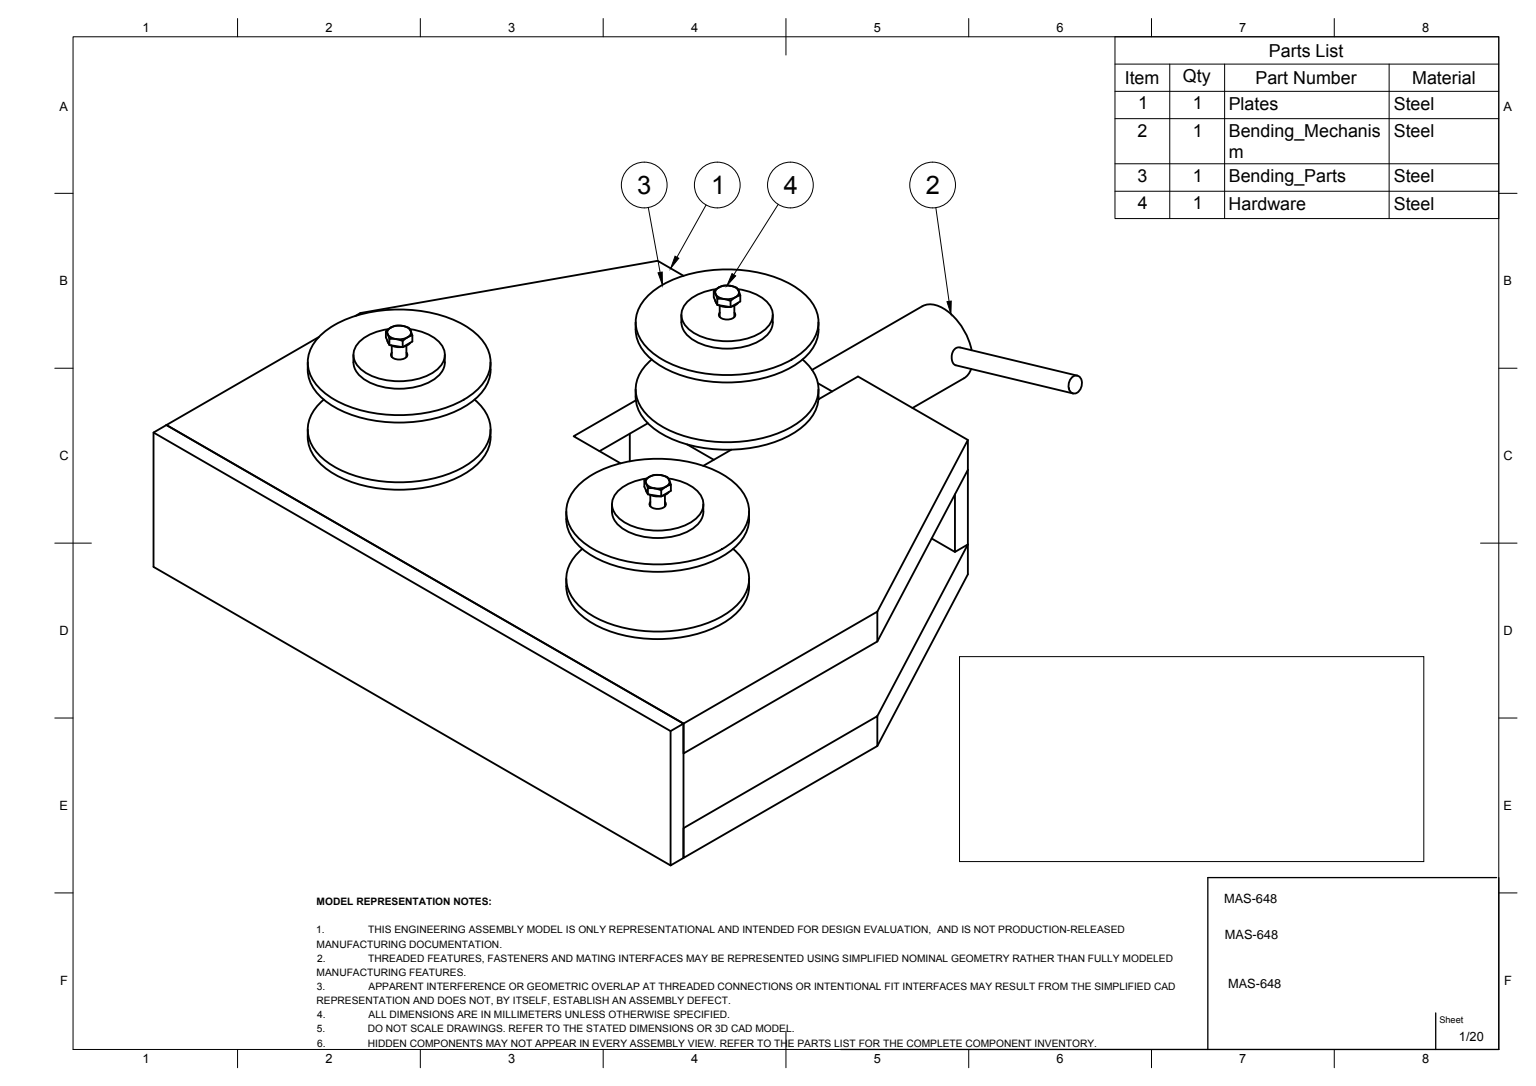
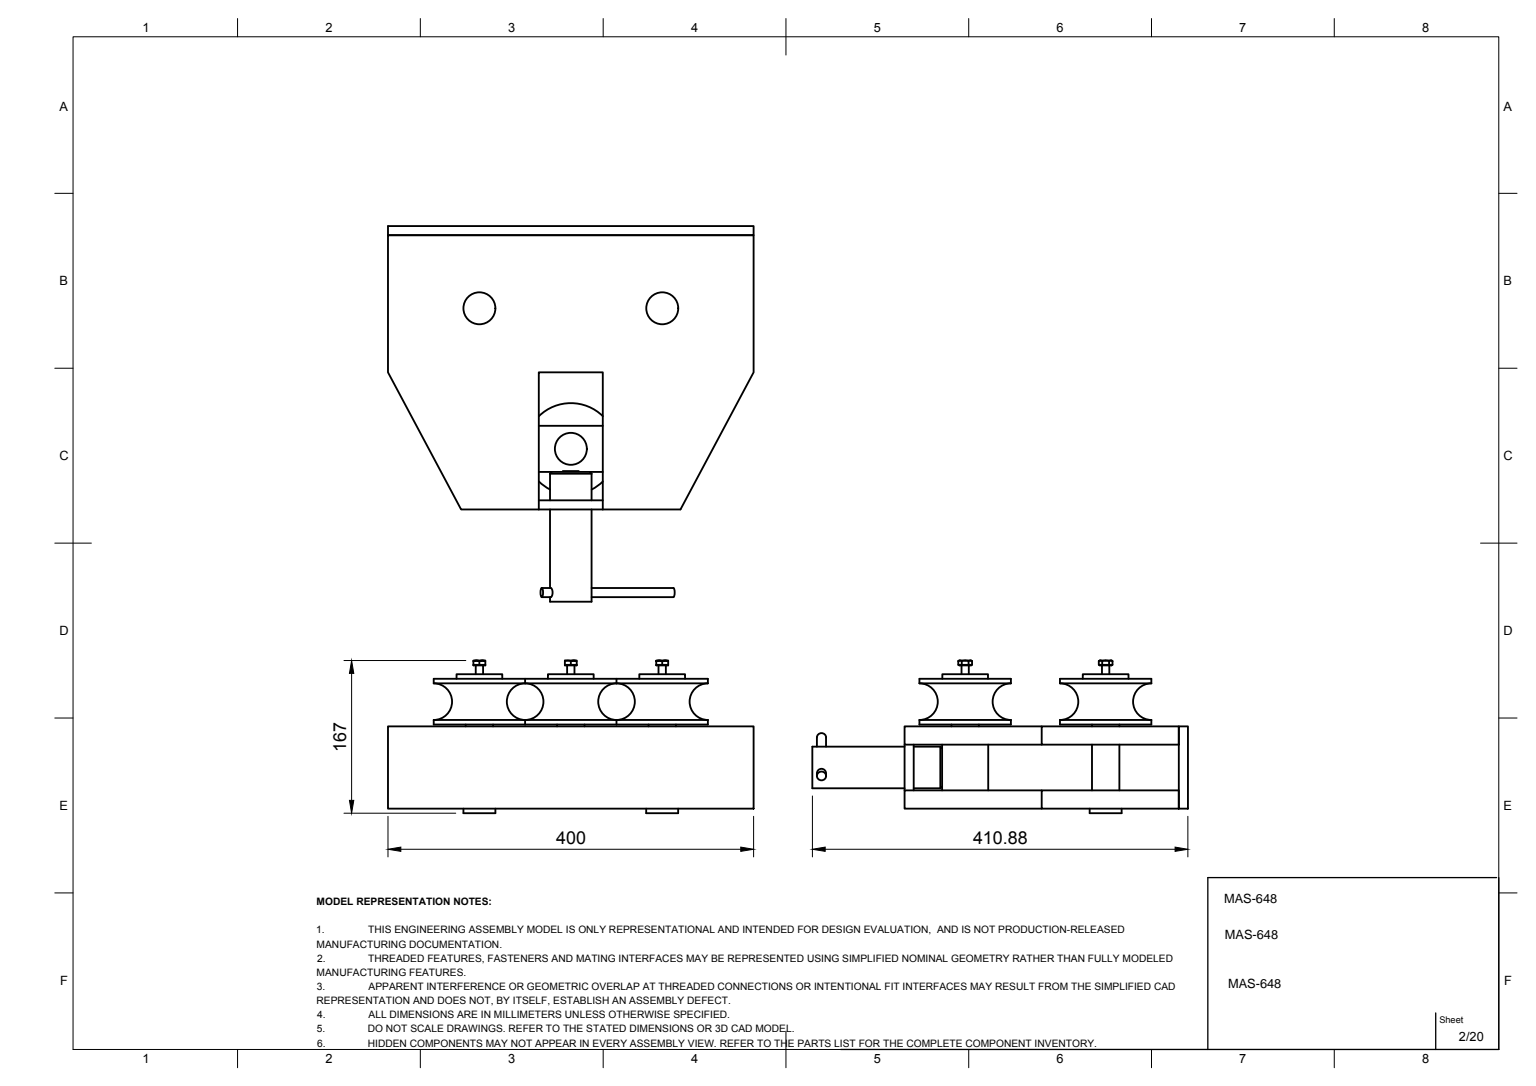
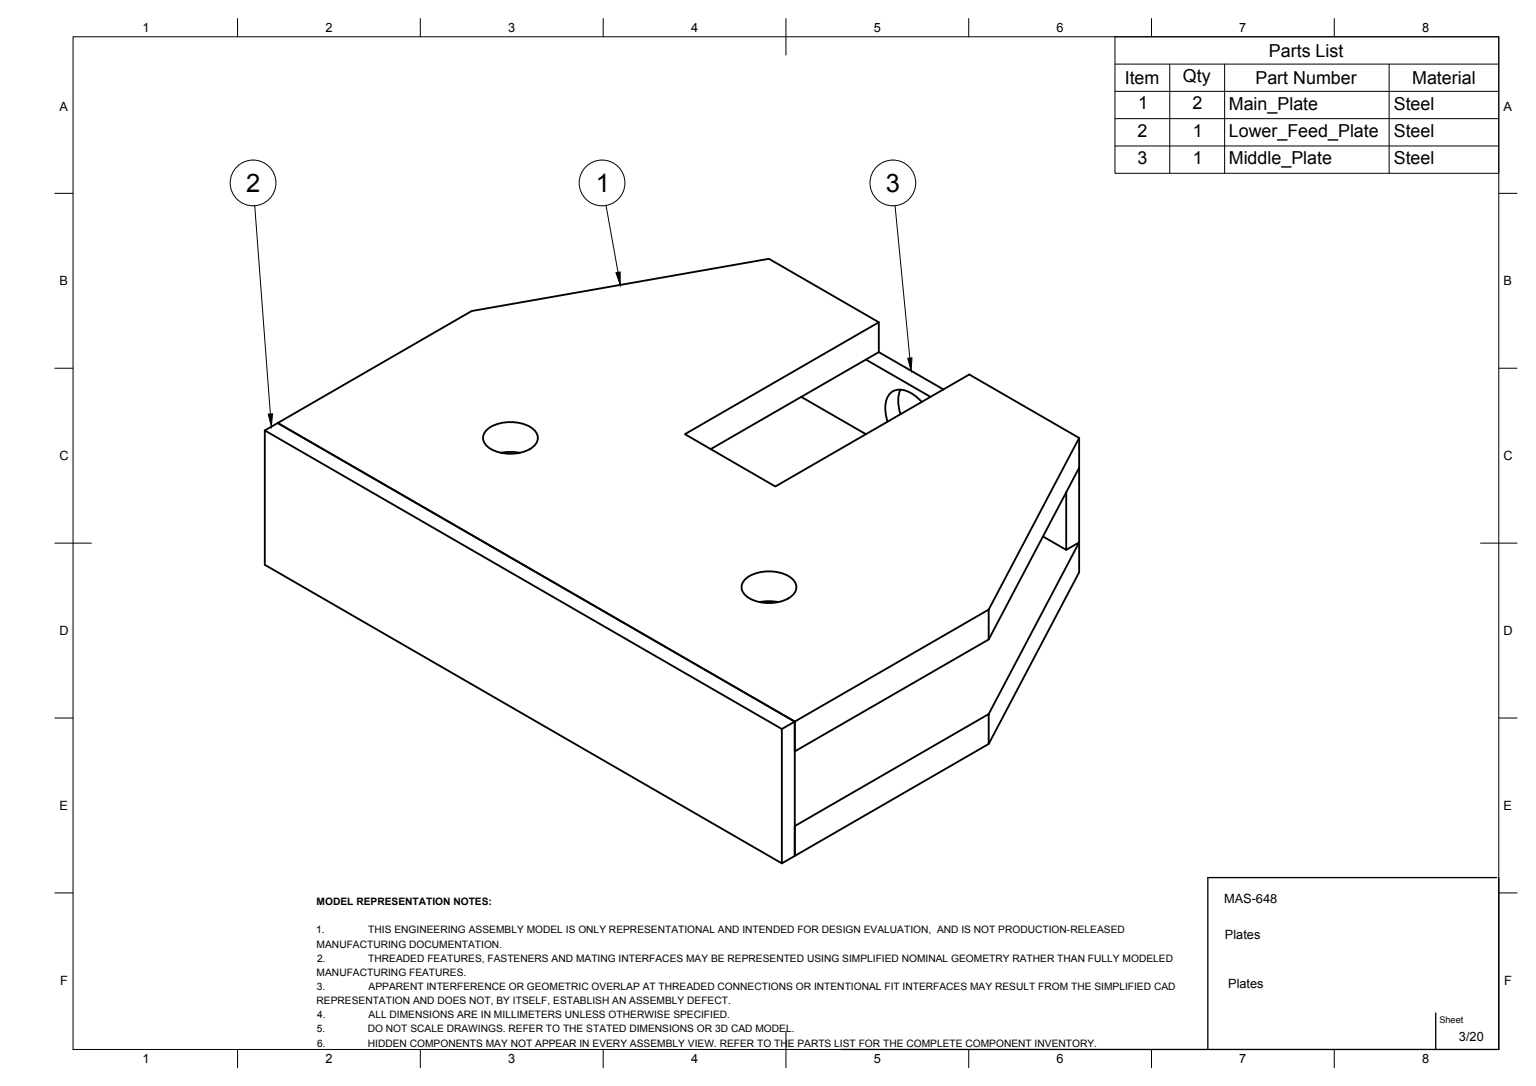
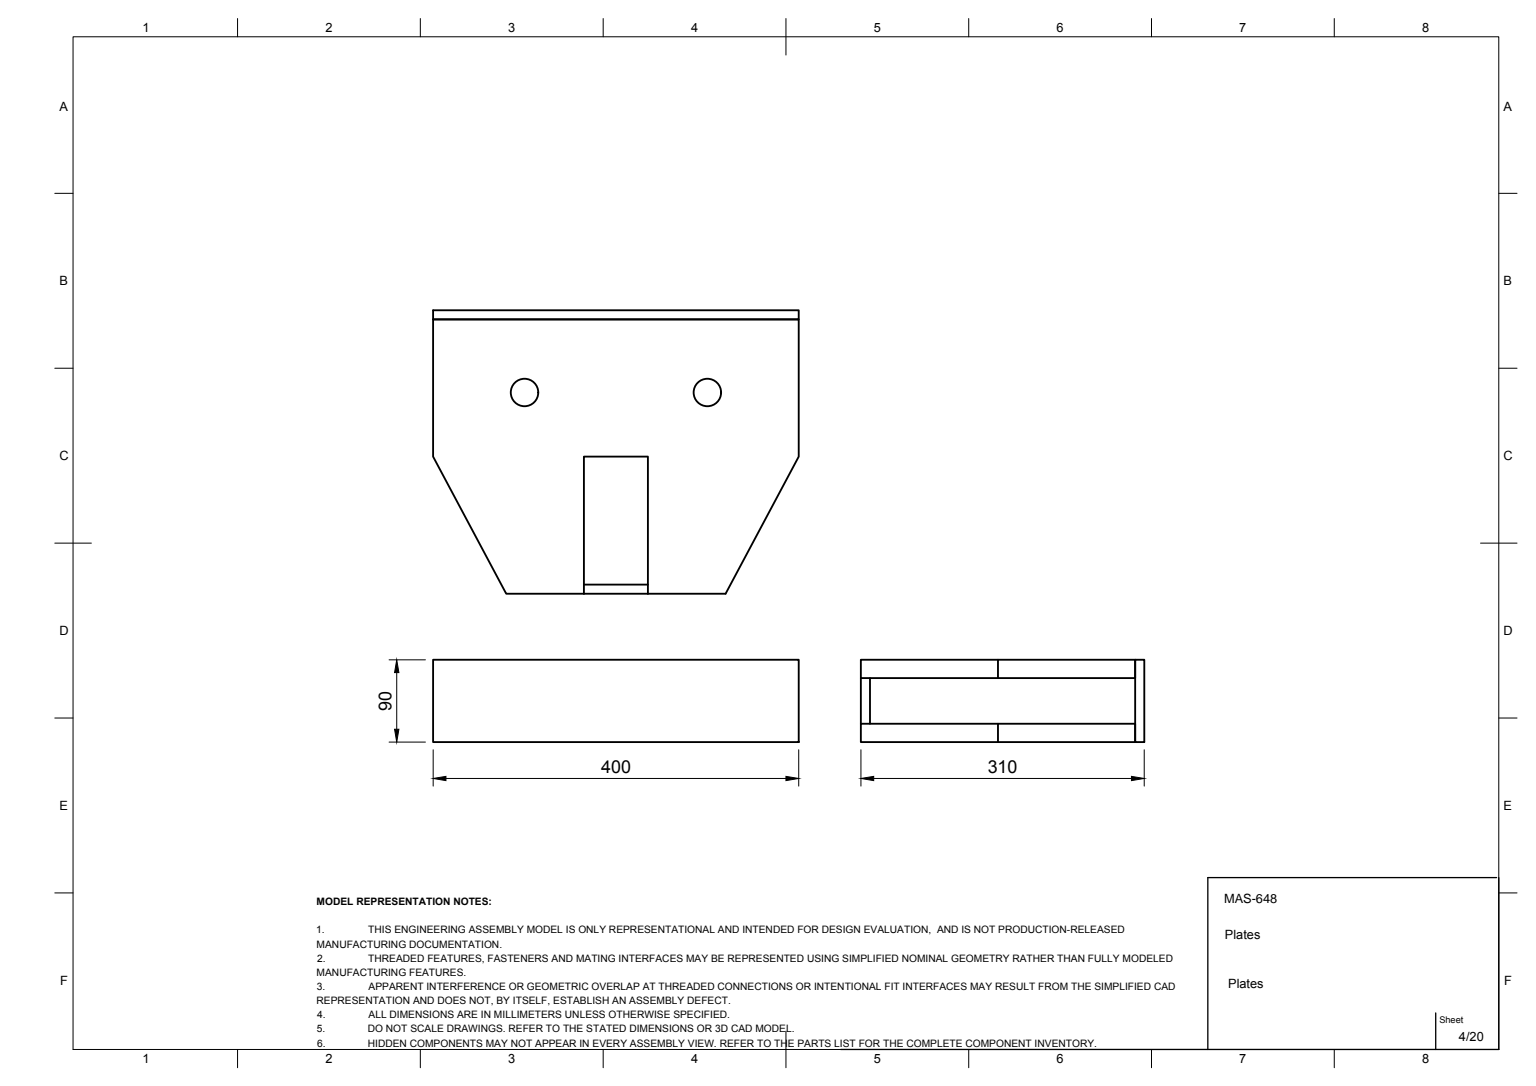
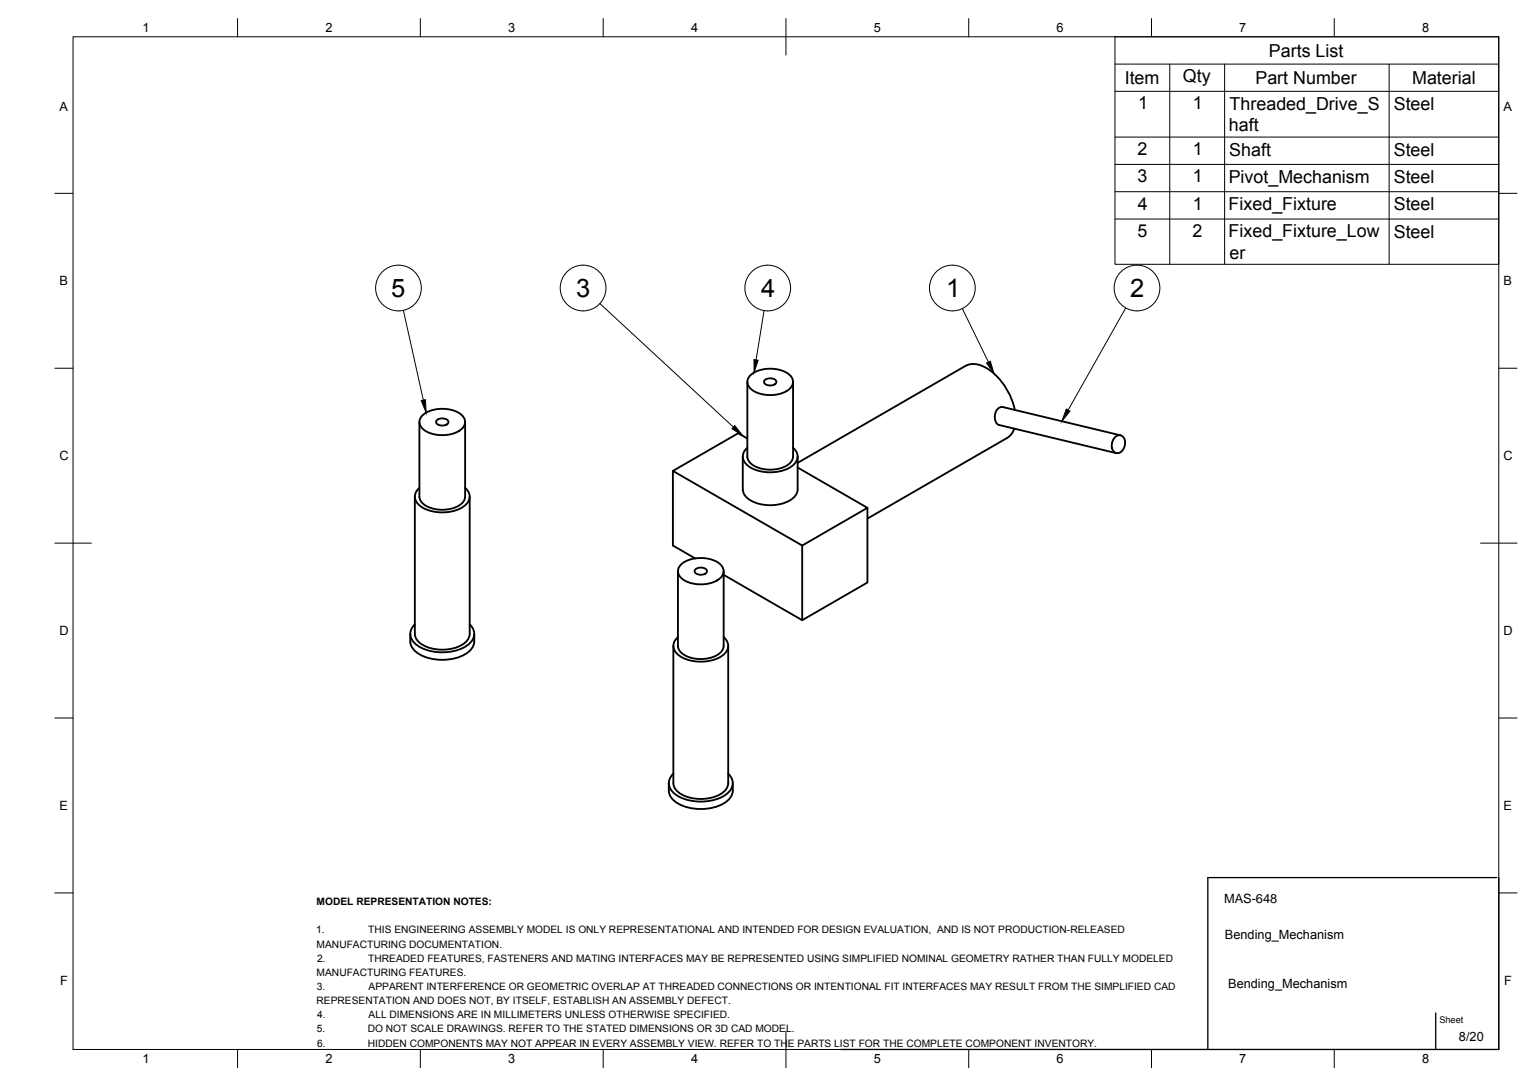
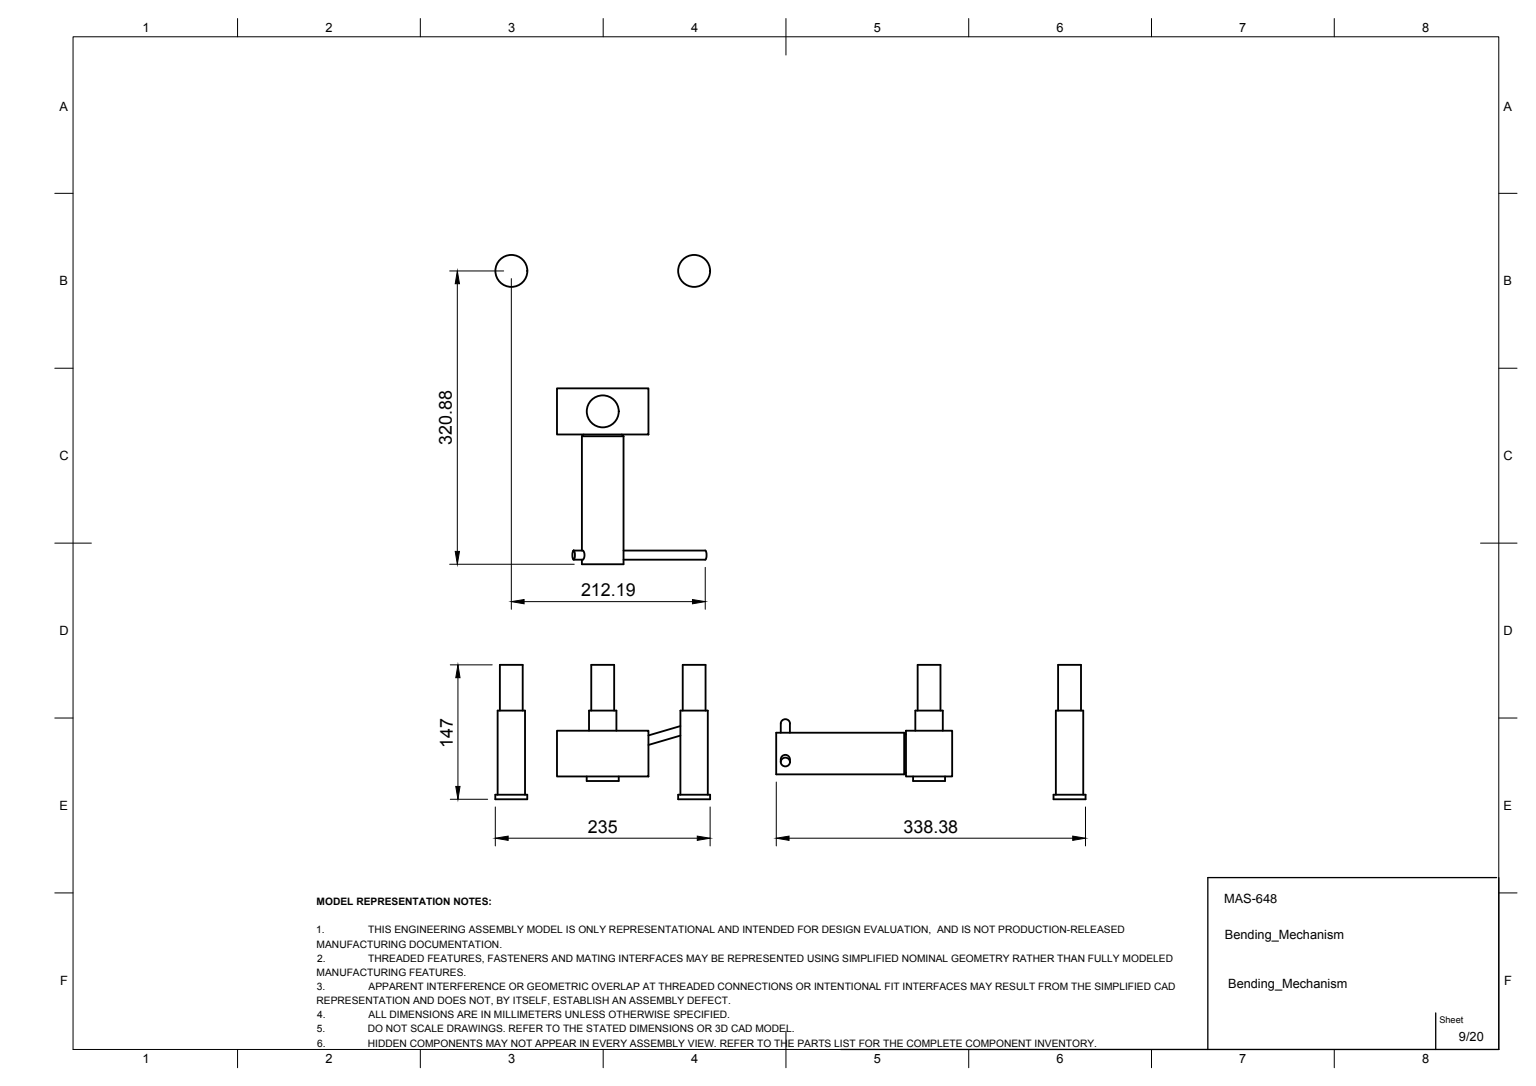
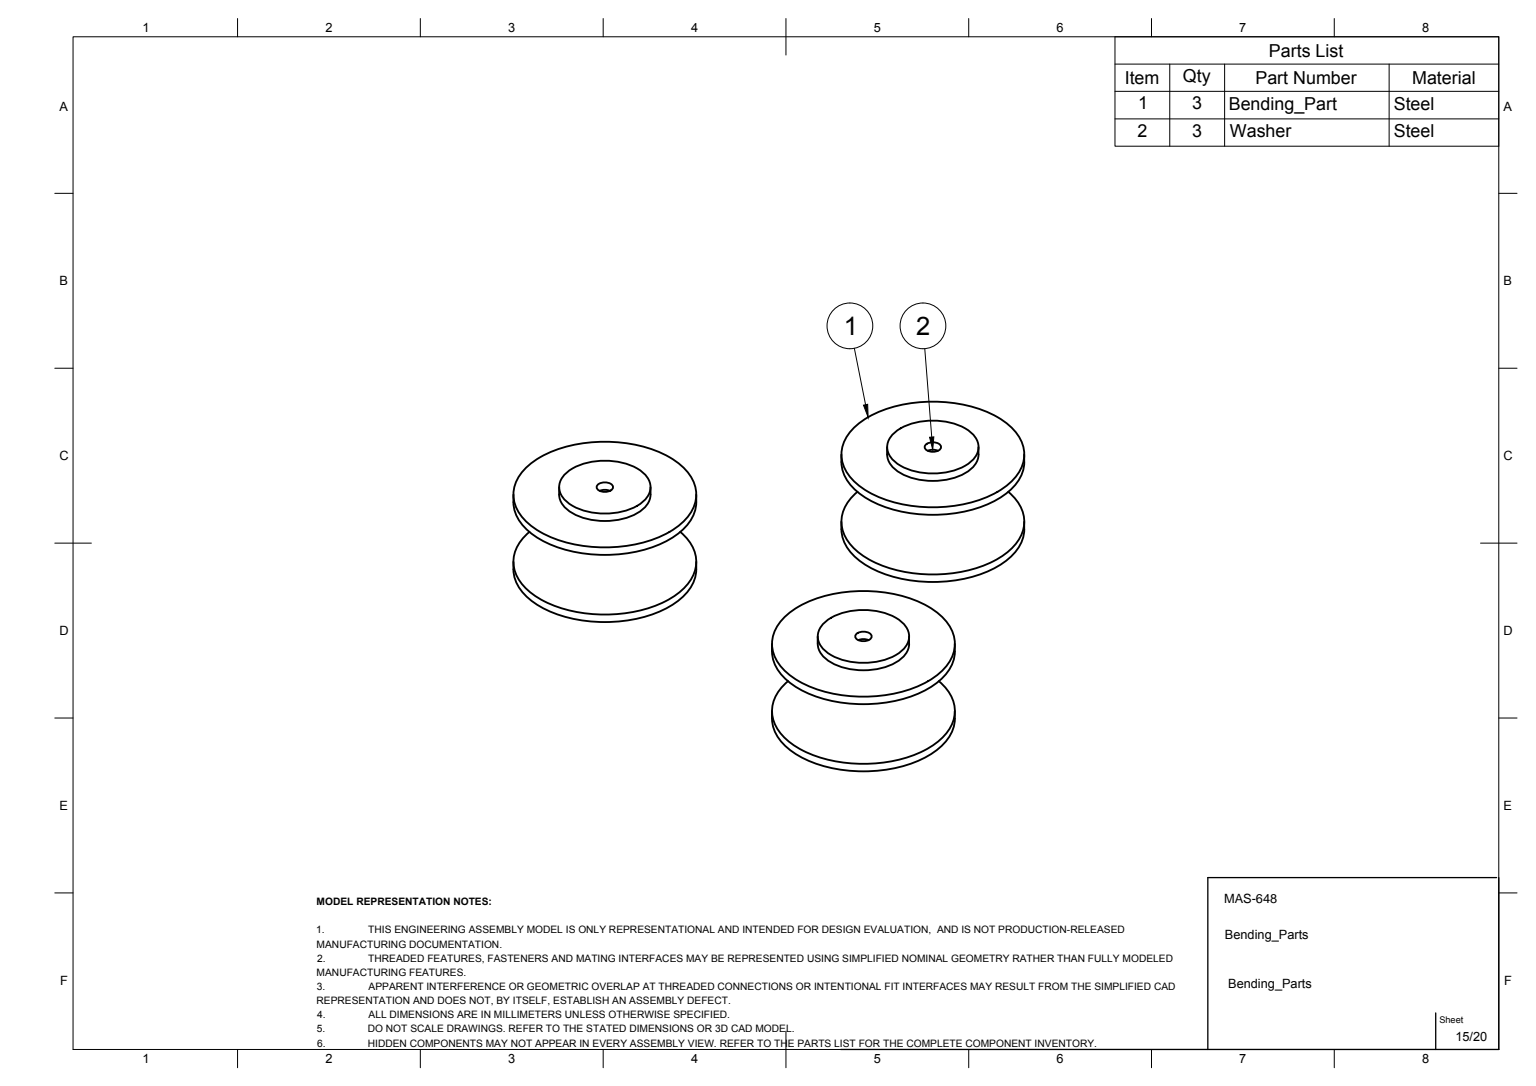
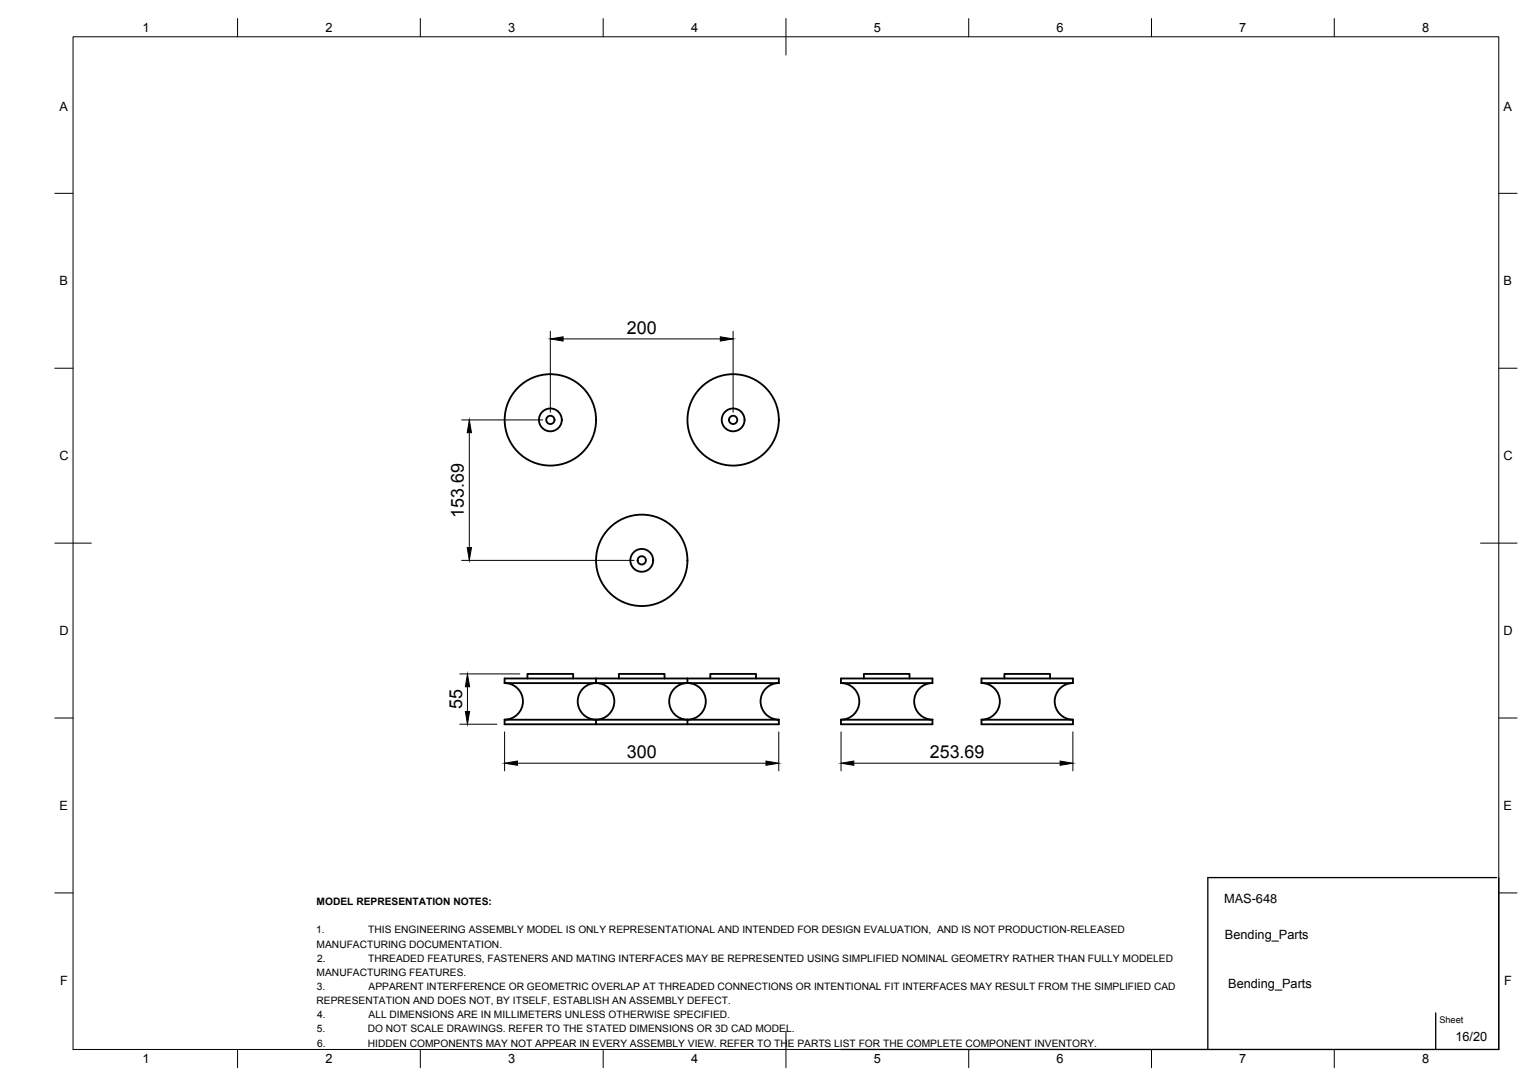
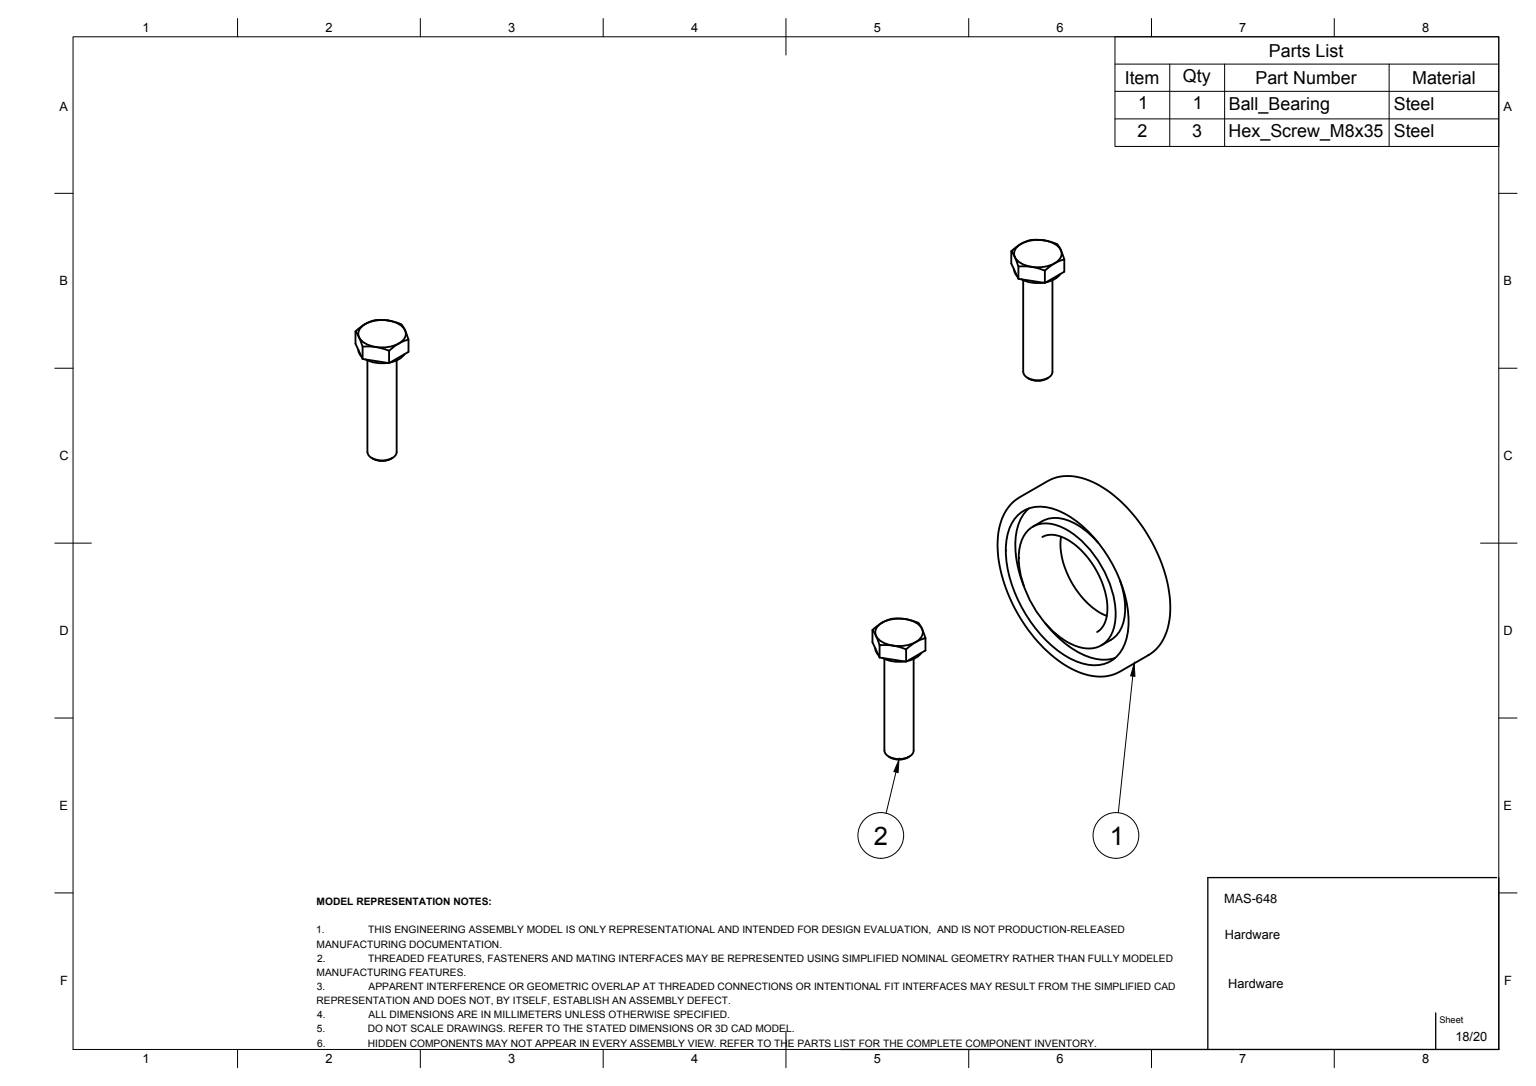
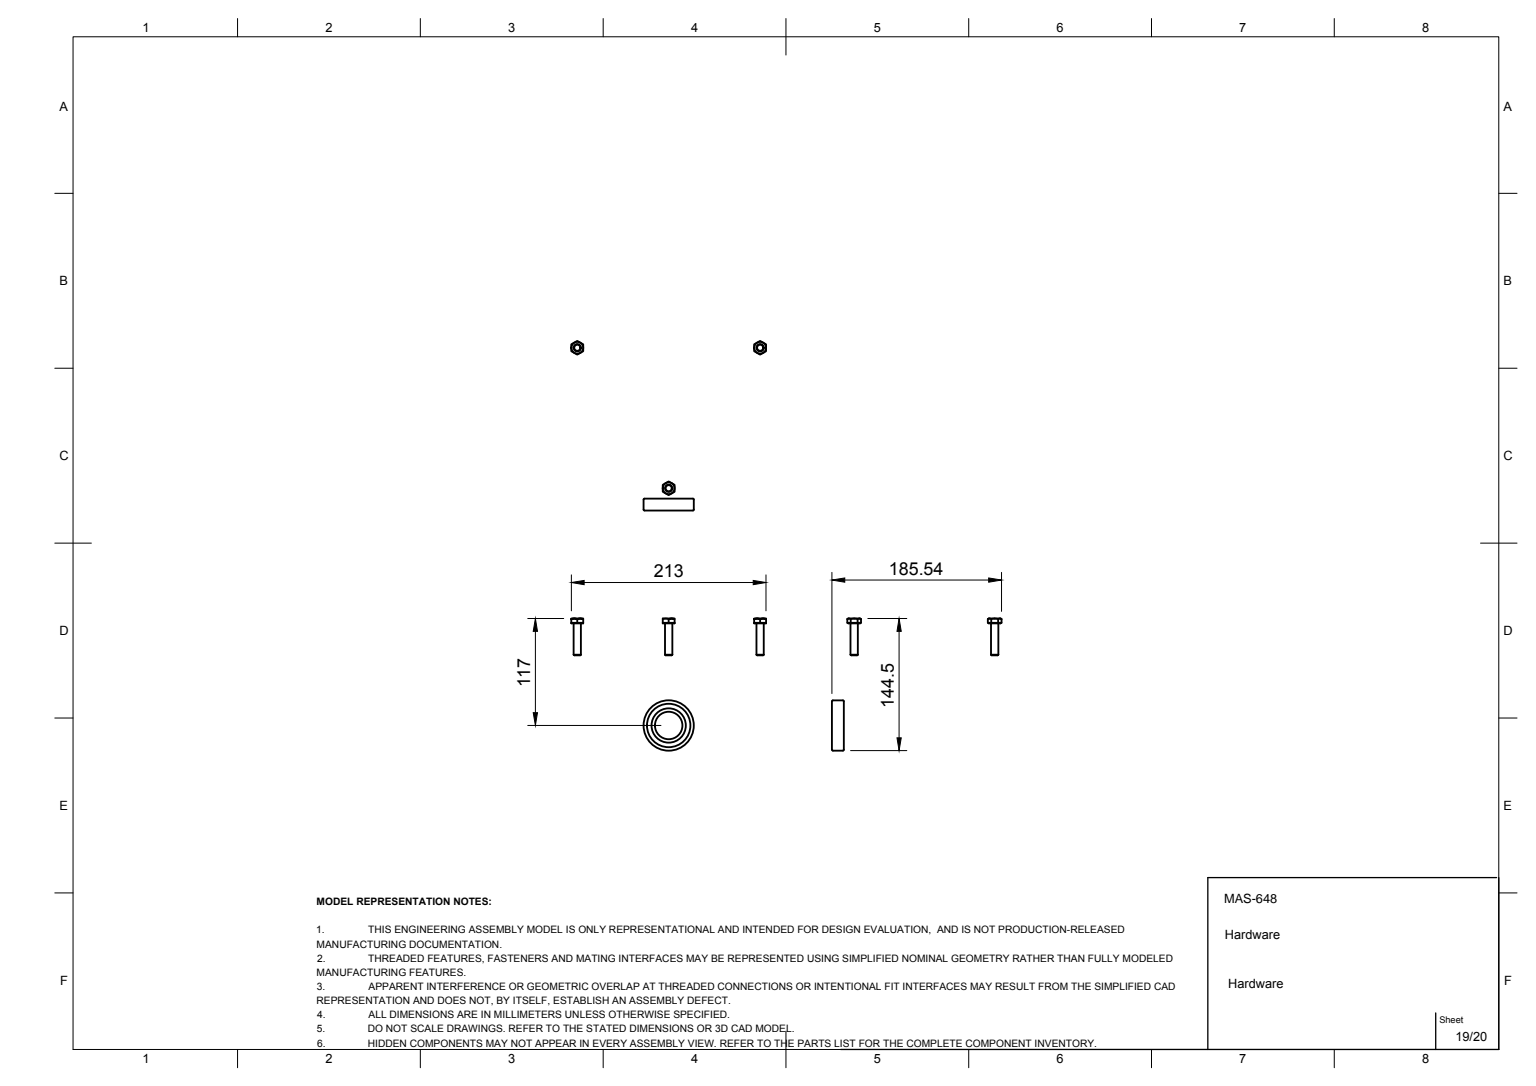
ISO-10303-21;
HEADER;
FILE_DESCRIPTION((''),'2;1');
FILE_NAME('MAS-648','2026-10-09T12:47:58-07:00',(''),(''),'','','');
FILE_SCHEMA (('AUTOMOTIVE_DESIGN { 1 0 10303 214 3 1 1 }'));
ENDSEC;
DATA;
#10 = MECHANICAL_DESIGN_GEOMETRIC_PRESENTATION_REPRESENTATION('',(#310,#311,
#312,#313,#314,#315,#316,#317,#318,#319,#320,#321),#3475) ;
#11 = (
BOUNDED_CURVE()
B_SPLINE_CURVE(2,(#3374,#3375,#3376),.UNSPECIFIED.,.F.,.F.)
B_SPLINE_CURVE_WITH_KNOTS((3,3),(-1.6071868741402,-0.951706480249473),
 .UNSPECIFIED.)
CURVE()
GEOMETRIC_REPRESENTATION_ITEM()
RATIONAL_B_SPLINE_CURVE((1.7594376617802,1.7594376617802,1.63311572113257))
REPRESENTATION_ITEM('')
) ;
#12 = (
BOUNDED_CURVE()
B_SPLINE_CURVE(2,(#3377,#3378,#3379),.UNSPECIFIED.,.F.,.F.)
B_SPLINE_CURVE_WITH_KNOTS((3,3),(-2.26266726803093,-1.6071868741402),
 .UNSPECIFIED.)
CURVE()
GEOMETRIC_REPRESENTATION_ITEM()
RATIONAL_B_SPLINE_CURVE((1.63311572113257,1.7594376617802,1.7594376617802))
REPRESENTATION_ITEM('')
) ;
#13 = (
BOUNDED_CURVE()
B_SPLINE_CURVE(2,(#3382,#3383,#3384),.UNSPECIFIED.,.F.,.F.)
B_SPLINE_CURVE_WITH_KNOTS((3,3),(-1.6071868741402,-0.951706480249475),
 .UNSPECIFIED.)
CURVE()
GEOMETRIC_REPRESENTATION_ITEM()
RATIONAL_B_SPLINE_CURVE((1.7594376617802,1.7594376617802,1.63311572113257))
REPRESENTATION_ITEM('')
) ;
#14 = (
BOUNDED_CURVE()
B_SPLINE_CURVE(2,(#3385,#3386,#3387),.UNSPECIFIED.,.F.,.F.)
B_SPLINE_CURVE_WITH_KNOTS((3,3),(-2.26266726803093,-1.6071868741402),
 .UNSPECIFIED.)
CURVE()
GEOMETRIC_REPRESENTATION_ITEM()
RATIONAL_B_SPLINE_CURVE((1.63311572113257,1.7594376617802,1.7594376617802))
REPRESENTATION_ITEM('')
) ;
#15 = (
BOUNDED_CURVE()
B_SPLINE_CURVE(2,(#3390,#3391,#3392),.UNSPECIFIED.,.F.,.F.)
B_SPLINE_CURVE_WITH_KNOTS((3,3),(-2.26266726803093,-1.6071868741402),
 .UNSPECIFIED.)
CURVE()
GEOMETRIC_REPRESENTATION_ITEM()
RATIONAL_B_SPLINE_CURVE((1.63311572113257,1.7594376617802,1.7594376617802))
REPRESENTATION_ITEM('')
) ;
#16 = (
BOUNDED_CURVE()
B_SPLINE_CURVE(2,(#3393,#3394,#3395),.UNSPECIFIED.,.F.,.F.)
B_SPLINE_CURVE_WITH_KNOTS((3,3),(-1.6071868741402,-0.951706480249475),
 .UNSPECIFIED.)
CURVE()
GEOMETRIC_REPRESENTATION_ITEM()
RATIONAL_B_SPLINE_CURVE((1.7594376617802,1.7594376617802,1.63311572113257))
REPRESENTATION_ITEM('')
) ;
#17 = (
BOUNDED_CURVE()
B_SPLINE_CURVE(2,(#3398,#3399,#3400),.UNSPECIFIED.,.F.,.F.)
B_SPLINE_CURVE_WITH_KNOTS((3,3),(-2.26266726803093,-1.6071868741402),
 .UNSPECIFIED.)
CURVE()
GEOMETRIC_REPRESENTATION_ITEM()
RATIONAL_B_SPLINE_CURVE((1.63311572113257,1.7594376617802,1.7594376617802))
REPRESENTATION_ITEM('')
) ;
#18 = (
BOUNDED_CURVE()
B_SPLINE_CURVE(2,(#3401,#3402,#3403),.UNSPECIFIED.,.F.,.F.)
B_SPLINE_CURVE_WITH_KNOTS((3,3),(-1.6071868741402,-0.951706480249475),
 .UNSPECIFIED.)
CURVE()
GEOMETRIC_REPRESENTATION_ITEM()
RATIONAL_B_SPLINE_CURVE((1.7594376617802,1.7594376617802,1.63311572113257))
REPRESENTATION_ITEM('')
) ;
#19 = (
BOUNDED_CURVE()
B_SPLINE_CURVE(2,(#3406,#3407,#3408),.UNSPECIFIED.,.F.,.F.)
B_SPLINE_CURVE_WITH_KNOTS((3,3),(-1.6071868741402,-0.951706480249475),
 .UNSPECIFIED.)
CURVE()
GEOMETRIC_REPRESENTATION_ITEM()
RATIONAL_B_SPLINE_CURVE((1.7594376617802,1.7594376617802,1.63311572113257))
REPRESENTATION_ITEM('')
) ;
#20 = (
BOUNDED_CURVE()
B_SPLINE_CURVE(2,(#3409,#3410,#3411),.UNSPECIFIED.,.F.,.F.)
B_SPLINE_CURVE_WITH_KNOTS((3,3),(-2.26266726803093,-1.6071868741402),
 .UNSPECIFIED.)
CURVE()
GEOMETRIC_REPRESENTATION_ITEM()
RATIONAL_B_SPLINE_CURVE((1.63311572113258,1.7594376617802,1.7594376617802))
REPRESENTATION_ITEM('')
) ;
#21 = (
BOUNDED_CURVE()
B_SPLINE_CURVE(2,(#3414,#3415,#3416),.UNSPECIFIED.,.F.,.F.)
B_SPLINE_CURVE_WITH_KNOTS((3,3),(-2.26266726803093,-1.6071868741402),
 .UNSPECIFIED.)
CURVE()
GEOMETRIC_REPRESENTATION_ITEM()
RATIONAL_B_SPLINE_CURVE((1.63311572113257,1.7594376617802,1.7594376617802))
REPRESENTATION_ITEM('')
) ;
#22 = (
BOUNDED_CURVE()
B_SPLINE_CURVE(2,(#3417,#3418,#3419),.UNSPECIFIED.,.F.,.F.)
B_SPLINE_CURVE_WITH_KNOTS((3,3),(-1.6071868741402,-0.951706480249472),
 .UNSPECIFIED.)
CURVE()
GEOMETRIC_REPRESENTATION_ITEM()
RATIONAL_B_SPLINE_CURVE((1.7594376617802,1.7594376617802,1.63311572113257))
REPRESENTATION_ITEM('')
) ;
#23 = TOROIDAL_SURFACE('',#2087,50.,20.) ;
#24 = TOROIDAL_SURFACE('',#2119,26.5,1.) ;
#25 = TOROIDAL_SURFACE('',#2125,26.5,1.) ;
#26 = TOROIDAL_SURFACE('',#2136,21.25,3.75) ;
#27 = TOROIDAL_SURFACE('',#2140,16.,1.) ;
#28 = TOROIDAL_SURFACE('',#2146,16.,1.) ;
#29 = TOROIDAL_SURFACE('',#2155,21.25,3.75) ;
#30 = TOROIDAL_SURFACE('',#2162,4.4,0.4) ;
#31 = CONICAL_SURFACE('',#2014,22.7551020408163,0.785398163397443) ;
#32 = CONICAL_SURFACE('',#2047,3.39999999999999,1.02974425867665) ;
#33 = CONICAL_SURFACE('',#2065,3.39999999999999,1.02974425867665) ;
#34 = CONICAL_SURFACE('',#2175,3.3095,0.785398163397441) ;
#35 = CONICAL_SURFACE('',#2194,6.5,1.0471975511966) ;
#36 = CONICAL_SURFACE('',#2195,6.5,1.0471975511966) ;
#37 = CONICAL_SURFACE('',#2196,6.5,1.0471975511966) ;
#38 = CONICAL_SURFACE('',#2197,6.5,1.0471975511966) ;
#39 = CONICAL_SURFACE('',#2198,6.5,1.0471975511966) ;
#40 = CONICAL_SURFACE('',#2199,6.5,1.0471975511966) ;
#41 = B_SPLINE_CURVE_WITH_KNOTS('',3,(#2969,#2970,#2971,#2972,#2973,#2974,
#2975,#2976,#2977,#2978,#2979,#2980,#2981,#2982,#2983,#2984,#2985,#2986,
#2987),.UNSPECIFIED.,.F.,.F.,(4,2,2,2,3,2,2,2,4),(-0.756034971359867,-0.567034005964369,
-0.378033040568871,-0.189016520284436,0.,0.189016520284436,0.378033040568871,
0.567034005964369,0.756034971359867),.UNSPECIFIED.) ;
#42 = B_SPLINE_CURVE_WITH_KNOTS('',3,(#2989,#2990,#2991,#2992,#2993,#2994,
#2995,#2996,#2997,#2998),.UNSPECIFIED.,.F.,.F.,(4,2,2,2,4),(0.756034971359867,
0.945035936755365,1.13403690215086,1.3230534224353,1.51206994271973),
 .UNSPECIFIED.) ;
#43 = B_SPLINE_CURVE_WITH_KNOTS('',3,(#3001,#3002,#3003,#3004,#3005,#3006,
#3007,#3008,#3009,#3010,#3011,#3012,#3013,#3014,#3015,#3016,#3017,#3018,
#3019,#3020,#3021,#3022,#3023,#3024,#3025,#3026,#3027,#3028,#3029,#3030,
#3031,#3032,#3033,#3034),.UNSPECIFIED.,.T.,.F.,(4,2,2,2,2,2,2,2,2,2,2,2,
2,2,2,2,4),(-3.02413988543947,-2.83512336515503,-2.6461068448706,-2.4571058794751,
-2.2681049140796,-2.0791039486841,-1.8901029832886,-1.70108646300417,-1.51206994271973,
-1.3230534224353,-1.13403690215086,-0.945035936755364,-0.756034971359867,
-0.567034005964369,-0.378033040568871,-0.189016520284436,0.),
 .UNSPECIFIED.) ;
#44 = B_SPLINE_CURVE_WITH_KNOTS('',3,(#3035,#3036,#3037,#3038,#3039,#3040,
#3041,#3042,#3043,#3044),.UNSPECIFIED.,.F.,.F.,(4,2,2,2,4),(1.51206994271973,
1.70108646300417,1.8901029832886,2.0791039486841,2.2681049140796),
 .UNSPECIFIED.) ;
#45 = ITEM_DEFINED_TRANSFORMATION($,$,#1988,#2007) ;
#46 = ITEM_DEFINED_TRANSFORMATION($,$,#1971,#2008) ;
#47 = ITEM_DEFINED_TRANSFORMATION($,$,#1978,#2009) ;
#48 = ITEM_DEFINED_TRANSFORMATION($,$,#1988,#2010) ;
#49 = ITEM_DEFINED_TRANSFORMATION($,$,#2012,#2079) ;
#50 = ITEM_DEFINED_TRANSFORMATION($,$,#2023,#2080) ;
#51 = ITEM_DEFINED_TRANSFORMATION($,$,#2029,#2081) ;
#52 = ITEM_DEFINED_TRANSFORMATION($,$,#2043,#2082) ;
#53 = ITEM_DEFINED_TRANSFORMATION($,$,#2061,#2083) ;
#54 = ITEM_DEFINED_TRANSFORMATION($,$,#2061,#2084) ;
#55 = ITEM_DEFINED_TRANSFORMATION($,$,#2086,#2111) ;
#56 = ITEM_DEFINED_TRANSFORMATION($,$,#2102,#2112) ;
#57 = ITEM_DEFINED_TRANSFORMATION($,$,#2086,#2113) ;
#58 = ITEM_DEFINED_TRANSFORMATION($,$,#2086,#2114) ;
#59 = ITEM_DEFINED_TRANSFORMATION($,$,#2102,#2115) ;
#60 = ITEM_DEFINED_TRANSFORMATION($,$,#2102,#2116) ;
#61 = ITEM_DEFINED_TRANSFORMATION($,$,#2118,#2206) ;
#62 = ITEM_DEFINED_TRANSFORMATION($,$,#2161,#2207) ;
#63 = ITEM_DEFINED_TRANSFORMATION($,$,#2161,#2208) ;
#64 = ITEM_DEFINED_TRANSFORMATION($,$,#2161,#2209) ;
#65 = ITEM_DEFINED_TRANSFORMATION($,$,#1970,#2210) ;
#66 = ITEM_DEFINED_TRANSFORMATION($,$,#2011,#2211) ;
#67 = ITEM_DEFINED_TRANSFORMATION($,$,#2085,#2212) ;
#68 = ITEM_DEFINED_TRANSFORMATION($,$,#2117,#2213) ;
#69 = (
REPRESENTATION_RELATIONSHIP($,$,#3542,#3539)
REPRESENTATION_RELATIONSHIP_WITH_TRANSFORMATION(#45)
SHAPE_REPRESENTATION_RELATIONSHIP()
) ;
#70 = (
REPRESENTATION_RELATIONSHIP($,$,#3540,#3539)
REPRESENTATION_RELATIONSHIP_WITH_TRANSFORMATION(#46)
SHAPE_REPRESENTATION_RELATIONSHIP()
) ;
#71 = (
REPRESENTATION_RELATIONSHIP($,$,#3541,#3539)
REPRESENTATION_RELATIONSHIP_WITH_TRANSFORMATION(#47)
SHAPE_REPRESENTATION_RELATIONSHIP()
) ;
#72 = (
REPRESENTATION_RELATIONSHIP($,$,#3542,#3539)
REPRESENTATION_RELATIONSHIP_WITH_TRANSFORMATION(#48)
SHAPE_REPRESENTATION_RELATIONSHIP()
) ;
#73 = (
REPRESENTATION_RELATIONSHIP($,$,#3544,#3543)
REPRESENTATION_RELATIONSHIP_WITH_TRANSFORMATION(#49)
SHAPE_REPRESENTATION_RELATIONSHIP()
) ;
#74 = (
REPRESENTATION_RELATIONSHIP($,$,#3545,#3543)
REPRESENTATION_RELATIONSHIP_WITH_TRANSFORMATION(#50)
SHAPE_REPRESENTATION_RELATIONSHIP()
) ;
#75 = (
REPRESENTATION_RELATIONSHIP($,$,#3546,#3543)
REPRESENTATION_RELATIONSHIP_WITH_TRANSFORMATION(#51)
SHAPE_REPRESENTATION_RELATIONSHIP()
) ;
#76 = (
REPRESENTATION_RELATIONSHIP($,$,#3547,#3543)
REPRESENTATION_RELATIONSHIP_WITH_TRANSFORMATION(#52)
SHAPE_REPRESENTATION_RELATIONSHIP()
) ;
#77 = (
REPRESENTATION_RELATIONSHIP($,$,#3548,#3543)
REPRESENTATION_RELATIONSHIP_WITH_TRANSFORMATION(#53)
SHAPE_REPRESENTATION_RELATIONSHIP()
) ;
#78 = (
REPRESENTATION_RELATIONSHIP($,$,#3548,#3543)
REPRESENTATION_RELATIONSHIP_WITH_TRANSFORMATION(#54)
SHAPE_REPRESENTATION_RELATIONSHIP()
) ;
#79 = (
REPRESENTATION_RELATIONSHIP($,$,#3550,#3549)
REPRESENTATION_RELATIONSHIP_WITH_TRANSFORMATION(#55)
SHAPE_REPRESENTATION_RELATIONSHIP()
) ;
#80 = (
REPRESENTATION_RELATIONSHIP($,$,#3551,#3549)
REPRESENTATION_RELATIONSHIP_WITH_TRANSFORMATION(#56)
SHAPE_REPRESENTATION_RELATIONSHIP()
) ;
#81 = (
REPRESENTATION_RELATIONSHIP($,$,#3550,#3549)
REPRESENTATION_RELATIONSHIP_WITH_TRANSFORMATION(#57)
SHAPE_REPRESENTATION_RELATIONSHIP()
) ;
#82 = (
REPRESENTATION_RELATIONSHIP($,$,#3550,#3549)
REPRESENTATION_RELATIONSHIP_WITH_TRANSFORMATION(#58)
SHAPE_REPRESENTATION_RELATIONSHIP()
) ;
#83 = (
REPRESENTATION_RELATIONSHIP($,$,#3551,#3549)
REPRESENTATION_RELATIONSHIP_WITH_TRANSFORMATION(#59)
SHAPE_REPRESENTATION_RELATIONSHIP()
) ;
#84 = (
REPRESENTATION_RELATIONSHIP($,$,#3551,#3549)
REPRESENTATION_RELATIONSHIP_WITH_TRANSFORMATION(#60)
SHAPE_REPRESENTATION_RELATIONSHIP()
) ;
#85 = (
REPRESENTATION_RELATIONSHIP($,$,#3553,#3552)
REPRESENTATION_RELATIONSHIP_WITH_TRANSFORMATION(#61)
SHAPE_REPRESENTATION_RELATIONSHIP()
) ;
#86 = (
REPRESENTATION_RELATIONSHIP($,$,#3554,#3552)
REPRESENTATION_RELATIONSHIP_WITH_TRANSFORMATION(#62)
SHAPE_REPRESENTATION_RELATIONSHIP()
) ;
#87 = (
REPRESENTATION_RELATIONSHIP($,$,#3554,#3552)
REPRESENTATION_RELATIONSHIP_WITH_TRANSFORMATION(#63)
SHAPE_REPRESENTATION_RELATIONSHIP()
) ;
#88 = (
REPRESENTATION_RELATIONSHIP($,$,#3554,#3552)
REPRESENTATION_RELATIONSHIP_WITH_TRANSFORMATION(#64)
SHAPE_REPRESENTATION_RELATIONSHIP()
) ;
#89 = (
REPRESENTATION_RELATIONSHIP($,$,#3539,#3538)
REPRESENTATION_RELATIONSHIP_WITH_TRANSFORMATION(#65)
SHAPE_REPRESENTATION_RELATIONSHIP()
) ;
#90 = (
REPRESENTATION_RELATIONSHIP($,$,#3543,#3538)
REPRESENTATION_RELATIONSHIP_WITH_TRANSFORMATION(#66)
SHAPE_REPRESENTATION_RELATIONSHIP()
) ;
#91 = (
REPRESENTATION_RELATIONSHIP($,$,#3549,#3538)
REPRESENTATION_RELATIONSHIP_WITH_TRANSFORMATION(#67)
SHAPE_REPRESENTATION_RELATIONSHIP()
) ;
#92 = (
REPRESENTATION_RELATIONSHIP($,$,#3552,#3538)
REPRESENTATION_RELATIONSHIP_WITH_TRANSFORMATION(#68)
SHAPE_REPRESENTATION_RELATIONSHIP()
) ;
#93 = CONTEXT_DEPENDENT_SHAPE_REPRESENTATION(#69,#3502) ;
#94 = CONTEXT_DEPENDENT_SHAPE_REPRESENTATION(#70,#3503) ;
#95 = CONTEXT_DEPENDENT_SHAPE_REPRESENTATION(#71,#3504) ;
#96 = CONTEXT_DEPENDENT_SHAPE_REPRESENTATION(#72,#3505) ;
#97 = CONTEXT_DEPENDENT_SHAPE_REPRESENTATION(#73,#3512) ;
#98 = CONTEXT_DEPENDENT_SHAPE_REPRESENTATION(#74,#3513) ;
#99 = CONTEXT_DEPENDENT_SHAPE_REPRESENTATION(#75,#3514) ;
#100 = CONTEXT_DEPENDENT_SHAPE_REPRESENTATION(#76,#3515) ;
#101 = CONTEXT_DEPENDENT_SHAPE_REPRESENTATION(#77,#3516) ;
#102 = CONTEXT_DEPENDENT_SHAPE_REPRESENTATION(#78,#3517) ;
#103 = CONTEXT_DEPENDENT_SHAPE_REPRESENTATION(#79,#3521) ;
#104 = CONTEXT_DEPENDENT_SHAPE_REPRESENTATION(#80,#3522) ;
#105 = CONTEXT_DEPENDENT_SHAPE_REPRESENTATION(#81,#3523) ;
#106 = CONTEXT_DEPENDENT_SHAPE_REPRESENTATION(#82,#3524) ;
#107 = CONTEXT_DEPENDENT_SHAPE_REPRESENTATION(#83,#3525) ;
#108 = CONTEXT_DEPENDENT_SHAPE_REPRESENTATION(#84,#3526) ;
#109 = CONTEXT_DEPENDENT_SHAPE_REPRESENTATION(#85,#3530) ;
#110 = CONTEXT_DEPENDENT_SHAPE_REPRESENTATION(#86,#3531) ;
#111 = CONTEXT_DEPENDENT_SHAPE_REPRESENTATION(#87,#3532) ;
#112 = CONTEXT_DEPENDENT_SHAPE_REPRESENTATION(#88,#3533) ;
#113 = CONTEXT_DEPENDENT_SHAPE_REPRESENTATION(#89,#3534) ;
#114 = CONTEXT_DEPENDENT_SHAPE_REPRESENTATION(#90,#3535) ;
#115 = CONTEXT_DEPENDENT_SHAPE_REPRESENTATION(#91,#3536) ;
#116 = CONTEXT_DEPENDENT_SHAPE_REPRESENTATION(#92,#3537) ;
#117 = NEXT_ASSEMBLY_USAGE_OCCURRENCE('Main_Plate:1','Main_Plate:1',
'Main_Plate:1',#3557,#3560,'Main_Plate:1') ;
#118 = NEXT_ASSEMBLY_USAGE_OCCURRENCE('Lower_Feed_Plate:1',
'Lower_Feed_Plate:1','Lower_Feed_Plate:1',#3557,#3558,
'Lower_Feed_Plate:1') ;
#119 = NEXT_ASSEMBLY_USAGE_OCCURRENCE('Middle_Plate:1','Middle_Plate:1',
'Middle_Plate:1',#3557,#3559,'Middle_Plate:1') ;
#120 = NEXT_ASSEMBLY_USAGE_OCCURRENCE('Main_Plate:2','Main_Plate:2',
'Main_Plate:2',#3557,#3560,'Main_Plate:2') ;
#121 = NEXT_ASSEMBLY_USAGE_OCCURRENCE('Threaded_Drive_Shaft:1',
'Threaded_Drive_Shaft:1','Threaded_Drive_Shaft:1',#3561,#3562,
'Threaded_Drive_Shaft:1') ;
#122 = NEXT_ASSEMBLY_USAGE_OCCURRENCE('Shaft:1','Shaft:1','Shaft:1',#3561,
#3563,'Shaft:1') ;
#123 = NEXT_ASSEMBLY_USAGE_OCCURRENCE('Pivot_Mechanism:1',
'Pivot_Mechanism:1','Pivot_Mechanism:1',#3561,#3564,'Pivot_Mechanism:1') ;
#124 = NEXT_ASSEMBLY_USAGE_OCCURRENCE('Fixed_Fixture:1','Fixed_Fixture:1',
'Fixed_Fixture:1',#3561,#3565,'Fixed_Fixture:1') ;
#125 = NEXT_ASSEMBLY_USAGE_OCCURRENCE('Fixed_Fixture_Lower:1',
'Fixed_Fixture_Lower:1','Fixed_Fixture_Lower:1',#3561,#3566,
'Fixed_Fixture_Lower:1') ;
#126 = NEXT_ASSEMBLY_USAGE_OCCURRENCE('Fixed_Fixture_Lower:2',
'Fixed_Fixture_Lower:2','Fixed_Fixture_Lower:2',#3561,#3566,
'Fixed_Fixture_Lower:2') ;
#127 = NEXT_ASSEMBLY_USAGE_OCCURRENCE('Bending_Part:1','Bending_Part:1',
'Bending_Part:1',#3567,#3568,'Bending_Part:1') ;
#128 = NEXT_ASSEMBLY_USAGE_OCCURRENCE('Washer:1','Washer:1','Washer:1',#3567,
#3569,'Washer:1') ;
#129 = NEXT_ASSEMBLY_USAGE_OCCURRENCE('Bending_Part:2','Bending_Part:2',
'Bending_Part:2',#3567,#3568,'Bending_Part:2') ;
#130 = NEXT_ASSEMBLY_USAGE_OCCURRENCE('Bending_Part:3','Bending_Part:3',
'Bending_Part:3',#3567,#3568,'Bending_Part:3') ;
#131 = NEXT_ASSEMBLY_USAGE_OCCURRENCE('Washer:2','Washer:2','Washer:2',#3567,
#3569,'Washer:2') ;
#132 = NEXT_ASSEMBLY_USAGE_OCCURRENCE('Washer:3','Washer:3','Washer:3',#3567,
#3569,'Washer:3') ;
#133 = NEXT_ASSEMBLY_USAGE_OCCURRENCE('Ball_Bearing:1','Ball_Bearing:1',
'Ball_Bearing:1',#3570,#3571,'Ball_Bearing:1') ;
#134 = NEXT_ASSEMBLY_USAGE_OCCURRENCE('Hex_Screw_M8x35:1',
'Hex_Screw_M8x35:1','Hex_Screw_M8x35:1',#3570,#3572,'Hex_Screw_M8x35:1') ;
#135 = NEXT_ASSEMBLY_USAGE_OCCURRENCE('Hex_Screw_M8x35:2',
'Hex_Screw_M8x35:2','Hex_Screw_M8x35:2',#3570,#3572,'Hex_Screw_M8x35:2') ;
#136 = NEXT_ASSEMBLY_USAGE_OCCURRENCE('Hex_Screw_M8x35:3',
'Hex_Screw_M8x35:3','Hex_Screw_M8x35:3',#3570,#3572,'Hex_Screw_M8x35:3') ;
#137 = NEXT_ASSEMBLY_USAGE_OCCURRENCE('Plates:1','Plates:1','Plates:1',#3556,
#3557,'Plates:1') ;
#138 = NEXT_ASSEMBLY_USAGE_OCCURRENCE('Bending_Mechanism:1',
'Bending_Mechanism:1','Bending_Mechanism:1',#3556,#3561,
'Bending_Mechanism:1') ;
#139 = NEXT_ASSEMBLY_USAGE_OCCURRENCE('Bending_Parts:1','Bending_Parts:1',
'Bending_Parts:1',#3556,#3567,'Bending_Parts:1') ;
#140 = NEXT_ASSEMBLY_USAGE_OCCURRENCE('Hardware:1','Hardware:1',
'Hardware:1',#3556,#3570,'Hardware:1') ;
#141 = FACE_BOUND('',#460,.T.) ;
#142 = FACE_BOUND('',#462,.T.) ;
#143 = FACE_BOUND('',#473,.T.) ;
#144 = FACE_BOUND('',#474,.T.) ;
#145 = FACE_BOUND('',#476,.T.) ;
#146 = FACE_BOUND('',#477,.T.) ;
#147 = FACE_BOUND('',#484,.T.) ;
#148 = FACE_BOUND('',#494,.T.) ;
#149 = FACE_BOUND('',#497,.T.) ;
#150 = FACE_BOUND('',#499,.T.) ;
#151 = FACE_BOUND('',#510,.T.) ;
#152 = FACE_BOUND('',#512,.T.) ;
#153 = FACE_BOUND('',#514,.T.) ;
#154 = FACE_BOUND('',#522,.T.) ;
#155 = FACE_BOUND('',#524,.T.) ;
#156 = FACE_BOUND('',#526,.T.) ;
#157 = FACE_BOUND('',#532,.T.) ;
#158 = FACE_BOUND('',#534,.T.) ;
#159 = FACE_BOUND('',#538,.T.) ;
#160 = FACE_BOUND('',#540,.T.) ;
#161 = FACE_BOUND('',#554,.T.) ;
#162 = FACE_BOUND('',#556,.T.) ;
#163 = FACE_BOUND('',#558,.T.) ;
#164 = FACE_BOUND('',#560,.T.) ;
#165 = FACE_BOUND('',#566,.T.) ;
#166 = CIRCLE('',#1980,20.) ;
#167 = CIRCLE('',#1981,20.) ;
#168 = CIRCLE('',#1990,15.) ;
#169 = CIRCLE('',#1991,15.) ;
#170 = CIRCLE('',#1993,15.) ;
#171 = CIRCLE('',#1994,15.) ;
#172 = CIRCLE('',#2015,22.7551020408163) ;
#173 = CIRCLE('',#2016,15.) ;
#174 = CIRCLE('',#2018,22.7551020408163) ;
#175 = CIRCLE('',#2020,15.) ;
#176 = CIRCLE('',#2025,5.) ;
#177 = CIRCLE('',#2026,5.) ;
#178 = CIRCLE('',#2031,15.) ;
#179 = CIRCLE('',#2032,15.) ;
#180 = CIRCLE('',#2034,15.) ;
#181 = CIRCLE('',#2035,15.) ;
#182 = CIRCLE('',#2045,3.39999999999999) ;
#183 = CIRCLE('',#2046,3.39999999999999) ;
#184 = CIRCLE('',#2049,12.5) ;
#185 = CIRCLE('',#2050,12.5) ;
#186 = CIRCLE('',#2052,15.) ;
#187 = CIRCLE('',#2053,15.) ;
#188 = CIRCLE('',#2055,17.5) ;
#189 = CIRCLE('',#2056,17.5) ;
#190 = CIRCLE('',#2063,3.39999999999999) ;
#191 = CIRCLE('',#2064,3.39999999999999) ;
#192 = CIRCLE('',#2067,12.5) ;
#193 = CIRCLE('',#2068,12.5) ;
#194 = CIRCLE('',#2070,15.) ;
#195 = CIRCLE('',#2071,15.) ;
#196 = CIRCLE('',#2073,17.5) ;
#197 = CIRCLE('',#2074,17.5) ;
#198 = CIRCLE('',#2088,50.) ;
#199 = CIRCLE('',#2089,20.) ;
#200 = CIRCLE('',#2090,50.) ;
#201 = CIRCLE('',#2091,50.) ;
#202 = CIRCLE('',#2092,50.) ;
#203 = CIRCLE('',#2094,12.5) ;
#204 = CIRCLE('',#2095,12.5) ;
#205 = CIRCLE('',#2097,50.) ;
#206 = CIRCLE('',#2099,50.) ;
#207 = CIRCLE('',#2104,4.5) ;
#208 = CIRCLE('',#2105,4.5) ;
#209 = CIRCLE('',#2107,25.) ;
#210 = CIRCLE('',#2108,25.) ;
#211 = CIRCLE('',#2120,27.5) ;
#212 = CIRCLE('',#2121,1.) ;
#213 = CIRCLE('',#2122,26.5) ;
#214 = CIRCLE('',#2124,27.5) ;
#215 = CIRCLE('',#2126,26.5) ;
#216 = CIRCLE('',#2127,1.) ;
#217 = CIRCLE('',#2129,23.75) ;
#218 = CIRCLE('',#2130,23.75) ;
#219 = CIRCLE('',#2131,23.75) ;
#220 = CIRCLE('',#2133,23.75) ;
#221 = CIRCLE('',#2134,23.75) ;
#222 = CIRCLE('',#2135,23.75) ;
#223 = CIRCLE('',#2137,18.75) ;
#224 = CIRCLE('',#2138,3.75) ;
#225 = CIRCLE('',#2139,18.75) ;
#226 = CIRCLE('',#2141,16.) ;
#227 = CIRCLE('',#2142,1.) ;
#228 = CIRCLE('',#2143,15.) ;
#229 = CIRCLE('',#2145,15.) ;
#230 = CIRCLE('',#2147,1.) ;
#231 = CIRCLE('',#2148,16.) ;
#232 = CIRCLE('',#2150,18.75) ;
#233 = CIRCLE('',#2152,18.75) ;
#234 = CIRCLE('',#2153,18.75) ;
#235 = CIRCLE('',#2154,18.75) ;
#236 = CIRCLE('',#2156,3.75) ;
#237 = CIRCLE('',#2163,4.) ;
#238 = CIRCLE('',#2164,4.) ;
#239 = CIRCLE('',#2165,0.4) ;
#240 = CIRCLE('',#2166,4.4) ;
#241 = CIRCLE('',#2168,6.5) ;
#242 = CIRCLE('',#2169,6.5) ;
#243 = CIRCLE('',#2170,6.5) ;
#244 = CIRCLE('',#2171,6.5) ;
#245 = CIRCLE('',#2172,6.5) ;
#246 = CIRCLE('',#2173,6.5) ;
#247 = CIRCLE('',#2174,6.5) ;
#248 = CIRCLE('',#2176,4.) ;
#249 = CIRCLE('',#2177,3.3095) ;
#250 = CIRCLE('',#2188,6.5) ;
#251 = CIRCLE('',#2189,6.5) ;
#252 = CIRCLE('',#2190,6.5) ;
#253 = CIRCLE('',#2191,6.5) ;
#254 = CIRCLE('',#2192,6.5) ;
#255 = CIRCLE('',#2193,6.5) ;
#256 = CYLINDRICAL_SURFACE('',#1979,20.) ;
#257 = CYLINDRICAL_SURFACE('',#1989,15.) ;
#258 = CYLINDRICAL_SURFACE('',#1992,15.) ;
#259 = CYLINDRICAL_SURFACE('',#2013,5.00000000000002) ;
#260 = CYLINDRICAL_SURFACE('',#2017,22.7551020408163) ;
#261 = CYLINDRICAL_SURFACE('',#2019,15.) ;
#262 = CYLINDRICAL_SURFACE('',#2024,5.) ;
#263 = CYLINDRICAL_SURFACE('',#2030,15.) ;
#264 = CYLINDRICAL_SURFACE('',#2033,15.) ;
#265 = CYLINDRICAL_SURFACE('',#2044,3.39999999999999) ;
#266 = CYLINDRICAL_SURFACE('',#2048,12.5) ;
#267 = CYLINDRICAL_SURFACE('',#2051,15.) ;
#268 = CYLINDRICAL_SURFACE('',#2054,17.5) ;
#269 = CYLINDRICAL_SURFACE('',#2062,3.39999999999999) ;
#270 = CYLINDRICAL_SURFACE('',#2066,12.5) ;
#271 = CYLINDRICAL_SURFACE('',#2069,15.) ;
#272 = CYLINDRICAL_SURFACE('',#2072,17.5) ;
#273 = CYLINDRICAL_SURFACE('',#2093,12.5) ;
#274 = CYLINDRICAL_SURFACE('',#2096,50.) ;
#275 = CYLINDRICAL_SURFACE('',#2098,50.) ;
#276 = CYLINDRICAL_SURFACE('',#2103,4.5) ;
#277 = CYLINDRICAL_SURFACE('',#2106,25.) ;
#278 = CYLINDRICAL_SURFACE('',#2123,27.5) ;
#279 = CYLINDRICAL_SURFACE('',#2128,23.75) ;
#280 = CYLINDRICAL_SURFACE('',#2132,23.75) ;
#281 = CYLINDRICAL_SURFACE('',#2144,15.) ;
#282 = CYLINDRICAL_SURFACE('',#2149,18.75) ;
#283 = CYLINDRICAL_SURFACE('',#2151,18.75) ;
#284 = CYLINDRICAL_SURFACE('',#2167,6.5) ;
#285 = CYLINDRICAL_SURFACE('',#2178,4.) ;
#286 = SHAPE_REPRESENTATION_RELATIONSHIP('SRR','None',#3540,#298) ;
#287 = SHAPE_REPRESENTATION_RELATIONSHIP('SRR','None',#3541,#299) ;
#288 = SHAPE_REPRESENTATION_RELATIONSHIP('SRR','None',#3542,#300) ;
#289 = SHAPE_REPRESENTATION_RELATIONSHIP('SRR','None',#3544,#301) ;
#290 = SHAPE_REPRESENTATION_RELATIONSHIP('SRR','None',#3545,#302) ;
#291 = SHAPE_REPRESENTATION_RELATIONSHIP('SRR','None',#3546,#303) ;
#292 = SHAPE_REPRESENTATION_RELATIONSHIP('SRR','None',#3547,#304) ;
#293 = SHAPE_REPRESENTATION_RELATIONSHIP('SRR','None',#3548,#305) ;
#294 = SHAPE_REPRESENTATION_RELATIONSHIP('SRR','None',#3550,#306) ;
#295 = SHAPE_REPRESENTATION_RELATIONSHIP('SRR','None',#3551,#307) ;
#296 = SHAPE_REPRESENTATION_RELATIONSHIP('SRR','None',#3553,#308) ;
#297 = SHAPE_REPRESENTATION_RELATIONSHIP('SRR','None',#3554,#309) ;
#298 = ADVANCED_BREP_SHAPE_REPRESENTATION('',(#322),#3460) ;
#299 = ADVANCED_BREP_SHAPE_REPRESENTATION('',(#323),#3461) ;
#300 = ADVANCED_BREP_SHAPE_REPRESENTATION('',(#324),#3462) ;
#301 = ADVANCED_BREP_SHAPE_REPRESENTATION('',(#325),#3464) ;
#302 = ADVANCED_BREP_SHAPE_REPRESENTATION('',(#326),#3465) ;
#303 = ADVANCED_BREP_SHAPE_REPRESENTATION('',(#327),#3466) ;
#304 = ADVANCED_BREP_SHAPE_REPRESENTATION('',(#328),#3467) ;
#305 = ADVANCED_BREP_SHAPE_REPRESENTATION('',(#329),#3468) ;
#306 = ADVANCED_BREP_SHAPE_REPRESENTATION('',(#330),#3470) ;
#307 = ADVANCED_BREP_SHAPE_REPRESENTATION('',(#331),#3471) ;
#308 = ADVANCED_BREP_SHAPE_REPRESENTATION('',(#332),#3473) ;
#309 = ADVANCED_BREP_SHAPE_REPRESENTATION('',(#333),#3474) ;
#310 = STYLED_ITEM('',(#3628),#322) ;
#311 = STYLED_ITEM('',(#3628),#323) ;
#312 = STYLED_ITEM('',(#3628),#324) ;
#313 = STYLED_ITEM('',(#3628),#325) ;
#314 = STYLED_ITEM('',(#3628),#326) ;
#315 = STYLED_ITEM('',(#3628),#327) ;
#316 = STYLED_ITEM('',(#3628),#328) ;
#317 = STYLED_ITEM('',(#3628),#329) ;
#318 = STYLED_ITEM('',(#3628),#330) ;
#319 = STYLED_ITEM('',(#3628),#331) ;
#320 = STYLED_ITEM('',(#3628),#332) ;
#321 = STYLED_ITEM('',(#3628),#333) ;
#322 = MANIFOLD_SOLID_BREP('Body1',#1824) ;
#323 = MANIFOLD_SOLID_BREP('Body1',#1825) ;
#324 = MANIFOLD_SOLID_BREP('Body1',#1826) ;
#325 = MANIFOLD_SOLID_BREP('Body1',#1827) ;
#326 = MANIFOLD_SOLID_BREP('Body1',#1828) ;
#327 = MANIFOLD_SOLID_BREP('Body1',#1829) ;
#328 = MANIFOLD_SOLID_BREP('Body1',#1830) ;
#329 = MANIFOLD_SOLID_BREP('Body1',#1831) ;
#330 = MANIFOLD_SOLID_BREP('Body1',#1832) ;
#331 = MANIFOLD_SOLID_BREP('Body1',#1833) ;
#332 = MANIFOLD_SOLID_BREP('Body1',#1834) ;
#333 = MANIFOLD_SOLID_BREP('Body1',#1835) ;
#334 = FACE_OUTER_BOUND('',#448,.T.) ;
#335 = FACE_OUTER_BOUND('',#449,.T.) ;
#336 = FACE_OUTER_BOUND('',#450,.T.) ;
#337 = FACE_OUTER_BOUND('',#451,.T.) ;
#338 = FACE_OUTER_BOUND('',#452,.T.) ;
#339 = FACE_OUTER_BOUND('',#453,.T.) ;
#340 = FACE_OUTER_BOUND('',#454,.T.) ;
#341 = FACE_OUTER_BOUND('',#455,.T.) ;
#342 = FACE_OUTER_BOUND('',#456,.T.) ;
#343 = FACE_OUTER_BOUND('',#457,.T.) ;
#344 = FACE_OUTER_BOUND('',#458,.T.) ;
#345 = FACE_OUTER_BOUND('',#459,.T.) ;
#346 = FACE_OUTER_BOUND('',#461,.T.) ;
#347 = FACE_OUTER_BOUND('',#463,.T.) ;
#348 = FACE_OUTER_BOUND('',#464,.T.) ;
#349 = FACE_OUTER_BOUND('',#465,.T.) ;
#350 = FACE_OUTER_BOUND('',#466,.T.) ;
#351 = FACE_OUTER_BOUND('',#467,.T.) ;
#352 = FACE_OUTER_BOUND('',#468,.T.) ;
#353 = FACE_OUTER_BOUND('',#469,.T.) ;
#354 = FACE_OUTER_BOUND('',#470,.T.) ;
#355 = FACE_OUTER_BOUND('',#471,.T.) ;
#356 = FACE_OUTER_BOUND('',#472,.T.) ;
#357 = FACE_OUTER_BOUND('',#475,.T.) ;
#358 = FACE_OUTER_BOUND('',#478,.T.) ;
#359 = FACE_OUTER_BOUND('',#479,.T.) ;
#360 = FACE_OUTER_BOUND('',#480,.T.) ;
#361 = FACE_OUTER_BOUND('',#481,.T.) ;
#362 = FACE_OUTER_BOUND('',#482,.T.) ;
#363 = FACE_OUTER_BOUND('',#483,.T.) ;
#364 = FACE_OUTER_BOUND('',#485,.T.) ;
#365 = FACE_OUTER_BOUND('',#486,.T.) ;
#366 = FACE_OUTER_BOUND('',#487,.T.) ;
#367 = FACE_OUTER_BOUND('',#488,.T.) ;
#368 = FACE_OUTER_BOUND('',#489,.T.) ;
#369 = FACE_OUTER_BOUND('',#490,.T.) ;
#370 = FACE_OUTER_BOUND('',#491,.T.) ;
#371 = FACE_OUTER_BOUND('',#492,.T.) ;
#372 = FACE_OUTER_BOUND('',#493,.T.) ;
#373 = FACE_OUTER_BOUND('',#495,.T.) ;
#374 = FACE_OUTER_BOUND('',#496,.T.) ;
#375 = FACE_OUTER_BOUND('',#498,.T.) ;
#376 = FACE_OUTER_BOUND('',#500,.T.) ;
#377 = FACE_OUTER_BOUND('',#501,.T.) ;
#378 = FACE_OUTER_BOUND('',#502,.T.) ;
#379 = FACE_OUTER_BOUND('',#503,.T.) ;
#380 = FACE_OUTER_BOUND('',#504,.T.) ;
#381 = FACE_OUTER_BOUND('',#505,.T.) ;
#382 = FACE_OUTER_BOUND('',#506,.T.) ;
#383 = FACE_OUTER_BOUND('',#507,.T.) ;
#384 = FACE_OUTER_BOUND('',#508,.T.) ;
#385 = FACE_OUTER_BOUND('',#509,.T.) ;
#386 = FACE_OUTER_BOUND('',#511,.T.) ;
#387 = FACE_OUTER_BOUND('',#513,.T.) ;
#388 = FACE_OUTER_BOUND('',#515,.T.) ;
#389 = FACE_OUTER_BOUND('',#516,.T.) ;
#390 = FACE_OUTER_BOUND('',#517,.T.) ;
#391 = FACE_OUTER_BOUND('',#518,.T.) ;
#392 = FACE_OUTER_BOUND('',#519,.T.) ;
#393 = FACE_OUTER_BOUND('',#520,.T.) ;
#394 = FACE_OUTER_BOUND('',#521,.T.) ;
#395 = FACE_OUTER_BOUND('',#523,.T.) ;
#396 = FACE_OUTER_BOUND('',#525,.T.) ;
#397 = FACE_OUTER_BOUND('',#527,.T.) ;
#398 = FACE_OUTER_BOUND('',#528,.T.) ;
#399 = FACE_OUTER_BOUND('',#529,.T.) ;
#400 = FACE_OUTER_BOUND('',#530,.T.) ;
#401 = FACE_OUTER_BOUND('',#531,.T.) ;
#402 = FACE_OUTER_BOUND('',#533,.T.) ;
#403 = FACE_OUTER_BOUND('',#535,.T.) ;
#404 = FACE_OUTER_BOUND('',#536,.T.) ;
#405 = FACE_OUTER_BOUND('',#537,.T.) ;
#406 = FACE_OUTER_BOUND('',#539,.T.) ;
#407 = FACE_OUTER_BOUND('',#541,.T.) ;
#408 = FACE_OUTER_BOUND('',#542,.T.) ;
#409 = FACE_OUTER_BOUND('',#543,.T.) ;
#410 = FACE_OUTER_BOUND('',#544,.T.) ;
#411 = FACE_OUTER_BOUND('',#545,.T.) ;
#412 = FACE_OUTER_BOUND('',#546,.T.) ;
#413 = FACE_OUTER_BOUND('',#547,.T.) ;
#414 = FACE_OUTER_BOUND('',#548,.T.) ;
#415 = FACE_OUTER_BOUND('',#549,.T.) ;
#416 = FACE_OUTER_BOUND('',#550,.T.) ;
#417 = FACE_OUTER_BOUND('',#551,.T.) ;
#418 = FACE_OUTER_BOUND('',#552,.T.) ;
#419 = FACE_OUTER_BOUND('',#553,.T.) ;
#420 = FACE_OUTER_BOUND('',#555,.T.) ;
#421 = FACE_OUTER_BOUND('',#557,.T.) ;
#422 = FACE_OUTER_BOUND('',#559,.T.) ;
#423 = FACE_OUTER_BOUND('',#561,.T.) ;
#424 = FACE_OUTER_BOUND('',#562,.T.) ;
#425 = FACE_OUTER_BOUND('',#563,.T.) ;
#426 = FACE_OUTER_BOUND('',#564,.T.) ;
#427 = FACE_OUTER_BOUND('',#565,.T.) ;
#428 = FACE_OUTER_BOUND('',#567,.T.) ;
#429 = FACE_OUTER_BOUND('',#568,.T.) ;
#430 = FACE_OUTER_BOUND('',#569,.T.) ;
#431 = FACE_OUTER_BOUND('',#570,.T.) ;
#432 = FACE_OUTER_BOUND('',#571,.T.) ;
#433 = FACE_OUTER_BOUND('',#572,.T.) ;
#434 = FACE_OUTER_BOUND('',#573,.T.) ;
#435 = FACE_OUTER_BOUND('',#574,.T.) ;
#436 = FACE_OUTER_BOUND('',#575,.T.) ;
#437 = FACE_OUTER_BOUND('',#576,.T.) ;
#438 = FACE_OUTER_BOUND('',#577,.T.) ;
#439 = FACE_OUTER_BOUND('',#578,.T.) ;
#440 = FACE_OUTER_BOUND('',#579,.T.) ;
#441 = FACE_OUTER_BOUND('',#580,.T.) ;
#442 = FACE_OUTER_BOUND('',#581,.T.) ;
#443 = FACE_OUTER_BOUND('',#582,.T.) ;
#444 = FACE_OUTER_BOUND('',#583,.T.) ;
#445 = FACE_OUTER_BOUND('',#584,.T.) ;
#446 = FACE_OUTER_BOUND('',#585,.T.) ;
#447 = FACE_OUTER_BOUND('',#586,.T.) ;
#448 = EDGE_LOOP('',(#1194,#1195,#1196,#1197)) ;
#449 = EDGE_LOOP('',(#1198,#1199,#1200,#1201)) ;
#450 = EDGE_LOOP('',(#1202,#1203,#1204,#1205)) ;
#451 = EDGE_LOOP('',(#1206,#1207,#1208,#1209)) ;
#452 = EDGE_LOOP('',(#1210,#1211,#1212,#1213)) ;
#453 = EDGE_LOOP('',(#1214,#1215,#1216,#1217)) ;
#454 = EDGE_LOOP('',(#1218,#1219,#1220,#1221)) ;
#455 = EDGE_LOOP('',(#1222,#1223,#1224,#1225)) ;
#456 = EDGE_LOOP('',(#1226,#1227,#1228,#1229)) ;
#457 = EDGE_LOOP('',(#1230,#1231,#1232,#1233)) ;
#458 = EDGE_LOOP('',(#1234,#1235,#1236,#1237)) ;
#459 = EDGE_LOOP('',(#1238,#1239,#1240,#1241)) ;
#460 = EDGE_LOOP('',(#1242)) ;
#461 = EDGE_LOOP('',(#1243,#1244,#1245,#1246)) ;
#462 = EDGE_LOOP('',(#1247)) ;
#463 = EDGE_LOOP('',(#1248,#1249,#1250,#1251)) ;
#464 = EDGE_LOOP('',(#1252,#1253,#1254,#1255)) ;
#465 = EDGE_LOOP('',(#1256,#1257,#1258,#1259)) ;
#466 = EDGE_LOOP('',(#1260,#1261,#1262,#1263)) ;
#467 = EDGE_LOOP('',(#1264,#1265,#1266,#1267)) ;
#468 = EDGE_LOOP('',(#1268,#1269,#1270,#1271)) ;
#469 = EDGE_LOOP('',(#1272,#1273,#1274,#1275)) ;
#470 = EDGE_LOOP('',(#1276,#1277,#1278,#1279)) ;
#471 = EDGE_LOOP('',(#1280,#1281,#1282,#1283)) ;
#472 = EDGE_LOOP('',(#1284,#1285,#1286,#1287,#1288,#1289,#1290,#1291,#1292,
#1293)) ;
#473 = EDGE_LOOP('',(#1294)) ;
#474 = EDGE_LOOP('',(#1295)) ;
#475 = EDGE_LOOP('',(#1296,#1297,#1298,#1299,#1300,#1301,#1302,#1303,#1304,
#1305)) ;
#476 = EDGE_LOOP('',(#1306)) ;
#477 = EDGE_LOOP('',(#1307)) ;
#478 = EDGE_LOOP('',(#1308,#1309,#1310,#1311)) ;
#479 = EDGE_LOOP('',(#1312,#1313,#1314,#1315)) ;
#480 = EDGE_LOOP('',(#1316,#1317,#1318,#1319)) ;
#481 = EDGE_LOOP('',(#1320,#1321,#1322,#1323,#1324,#1325)) ;
#482 = EDGE_LOOP('',(#1326,#1327,#1328,#1329)) ;
#483 = EDGE_LOOP('',(#1330,#1331,#1332,#1333,#1334,#1335,#1336,#1337,#1338)) ;
#484 = EDGE_LOOP('',(#1339)) ;
#485 = EDGE_LOOP('',(#1340,#1341,#1342,#1343)) ;
#486 = EDGE_LOOP('',(#1344)) ;
#487 = EDGE_LOOP('',(#1345)) ;
#488 = EDGE_LOOP('',(#1346,#1347,#1348,#1349)) ;
#489 = EDGE_LOOP('',(#1350)) ;
#490 = EDGE_LOOP('',(#1351)) ;
#491 = EDGE_LOOP('',(#1352,#1353,#1354,#1355)) ;
#492 = EDGE_LOOP('',(#1356,#1357,#1358,#1359)) ;
#493 = EDGE_LOOP('',(#1360,#1361,#1362,#1363)) ;
#494 = EDGE_LOOP('',(#1364)) ;
#495 = EDGE_LOOP('',(#1365,#1366,#1367,#1368)) ;
#496 = EDGE_LOOP('',(#1369,#1370,#1371,#1372)) ;
#497 = EDGE_LOOP('',(#1373)) ;
#498 = EDGE_LOOP('',(#1374,#1375,#1376,#1377)) ;
#499 = EDGE_LOOP('',(#1378)) ;
#500 = EDGE_LOOP('',(#1379,#1380,#1381,#1382)) ;
#501 = EDGE_LOOP('',(#1383,#1384,#1385,#1386)) ;
#502 = EDGE_LOOP('',(#1387)) ;
#503 = EDGE_LOOP('',(#1388,#1389,#1390,#1391)) ;
#504 = EDGE_LOOP('',(#1392,#1393,#1394)) ;
#505 = EDGE_LOOP('',(#1395,#1396,#1397,#1398)) ;
#506 = EDGE_LOOP('',(#1399,#1400,#1401,#1402)) ;
#507 = EDGE_LOOP('',(#1403,#1404,#1405,#1406)) ;
#508 = EDGE_LOOP('',(#1407)) ;
#509 = EDGE_LOOP('',(#1408)) ;
#510 = EDGE_LOOP('',(#1409)) ;
#511 = EDGE_LOOP('',(#1410)) ;
#512 = EDGE_LOOP('',(#1411)) ;
#513 = EDGE_LOOP('',(#1412)) ;
#514 = EDGE_LOOP('',(#1413)) ;
#515 = EDGE_LOOP('',(#1414,#1415,#1416,#1417)) ;
#516 = EDGE_LOOP('',(#1418,#1419,#1420)) ;
#517 = EDGE_LOOP('',(#1421,#1422,#1423,#1424)) ;
#518 = EDGE_LOOP('',(#1425,#1426,#1427,#1428)) ;
#519 = EDGE_LOOP('',(#1429,#1430,#1431,#1432)) ;
#520 = EDGE_LOOP('',(#1433)) ;
#521 = EDGE_LOOP('',(#1434)) ;
#522 = EDGE_LOOP('',(#1435)) ;
#523 = EDGE_LOOP('',(#1436)) ;
#524 = EDGE_LOOP('',(#1437)) ;
#525 = EDGE_LOOP('',(#1438)) ;
#526 = EDGE_LOOP('',(#1439)) ;
#527 = EDGE_LOOP('',(#1440,#1441,#1442,#1443,#1444,#1445)) ;
#528 = EDGE_LOOP('',(#1446,#1447,#1448,#1449)) ;
#529 = EDGE_LOOP('',(#1450,#1451,#1452,#1453,#1454)) ;
#530 = EDGE_LOOP('',(#1455,#1456,#1457,#1458,#1459)) ;
#531 = EDGE_LOOP('',(#1460)) ;
#532 = EDGE_LOOP('',(#1461)) ;
#533 = EDGE_LOOP('',(#1462)) ;
#534 = EDGE_LOOP('',(#1463)) ;
#535 = EDGE_LOOP('',(#1464,#1465,#1466,#1467)) ;
#536 = EDGE_LOOP('',(#1468,#1469,#1470,#1471)) ;
#537 = EDGE_LOOP('',(#1472)) ;
#538 = EDGE_LOOP('',(#1473)) ;
#539 = EDGE_LOOP('',(#1474)) ;
#540 = EDGE_LOOP('',(#1475)) ;
#541 = EDGE_LOOP('',(#1476,#1477,#1478,#1479)) ;
#542 = EDGE_LOOP('',(#1480,#1481,#1482,#1483)) ;
#543 = EDGE_LOOP('',(#1484,#1485,#1486,#1487)) ;
#544 = EDGE_LOOP('',(#1488,#1489,#1490,#1491,#1492)) ;
#545 = EDGE_LOOP('',(#1493,#1494,#1495,#1496,#1497)) ;
#546 = EDGE_LOOP('',(#1498,#1499,#1500,#1501,#1502,#1503)) ;
#547 = EDGE_LOOP('',(#1504,#1505,#1506,#1507)) ;
#548 = EDGE_LOOP('',(#1508,#1509,#1510,#1511)) ;
#549 = EDGE_LOOP('',(#1512,#1513,#1514,#1515)) ;
#550 = EDGE_LOOP('',(#1516,#1517,#1518,#1519,#1520)) ;
#551 = EDGE_LOOP('',(#1521,#1522,#1523,#1524,#1525)) ;
#552 = EDGE_LOOP('',(#1526,#1527,#1528,#1529,#1530,#1531)) ;
#553 = EDGE_LOOP('',(#1532)) ;
#554 = EDGE_LOOP('',(#1533)) ;
#555 = EDGE_LOOP('',(#1534)) ;
#556 = EDGE_LOOP('',(#1535)) ;
#557 = EDGE_LOOP('',(#1536)) ;
#558 = EDGE_LOOP('',(#1537)) ;
#559 = EDGE_LOOP('',(#1538)) ;
#560 = EDGE_LOOP('',(#1539)) ;
#561 = EDGE_LOOP('',(#1540,#1541,#1542,#1543,#1544)) ;
#562 = EDGE_LOOP('',(#1545,#1546,#1547,#1548,#1549,#1550,#1551,#1552,#1553)) ;
#563 = EDGE_LOOP('',(#1554,#1555,#1556,#1557)) ;
#564 = EDGE_LOOP('',(#1558,#1559,#1560,#1561,#1562)) ;
#565 = EDGE_LOOP('',(#1563)) ;
#566 = EDGE_LOOP('',(#1564)) ;
#567 = EDGE_LOOP('',(#1565)) ;
#568 = EDGE_LOOP('',(#1566,#1567,#1568)) ;
#569 = EDGE_LOOP('',(#1569,#1570,#1571)) ;
#570 = EDGE_LOOP('',(#1572,#1573,#1574)) ;
#571 = EDGE_LOOP('',(#1575,#1576,#1577)) ;
#572 = EDGE_LOOP('',(#1578,#1579,#1580)) ;
#573 = EDGE_LOOP('',(#1581,#1582,#1583)) ;
#574 = EDGE_LOOP('',(#1584,#1585,#1586,#1587,#1588,#1589)) ;
#575 = EDGE_LOOP('',(#1590,#1591,#1592)) ;
#576 = EDGE_LOOP('',(#1593,#1594,#1595)) ;
#577 = EDGE_LOOP('',(#1596,#1597,#1598)) ;
#578 = EDGE_LOOP('',(#1599,#1600,#1601)) ;
#579 = EDGE_LOOP('',(#1602,#1603,#1604)) ;
#580 = EDGE_LOOP('',(#1605,#1606,#1607)) ;
#581 = EDGE_LOOP('',(#1608,#1609,#1610,#1611,#1612,#1613)) ;
#582 = EDGE_LOOP('',(#1614,#1615,#1616,#1617,#1618,#1619)) ;
#583 = EDGE_LOOP('',(#1620,#1621,#1622,#1623,#1624,#1625)) ;
#584 = EDGE_LOOP('',(#1626,#1627,#1628,#1629,#1630,#1631)) ;
#585 = EDGE_LOOP('',(#1632,#1633,#1634,#1635,#1636,#1637)) ;
#586 = EDGE_LOOP('',(#1638,#1639,#1640,#1641,#1642,#1643)) ;
#587 = LINE('',#2829,#706) ;
#588 = LINE('',#2831,#707) ;
#589 = LINE('',#2833,#708) ;
#590 = LINE('',#2834,#709) ;
#591 = LINE('',#2837,#710) ;
#592 = LINE('',#2839,#711) ;
#593 = LINE('',#2840,#712) ;
#594 = LINE('',#2843,#713) ;
#595 = LINE('',#2845,#714) ;
#596 = LINE('',#2846,#715) ;
#597 = LINE('',#2848,#716) ;
#598 = LINE('',#2849,#717) ;
#599 = LINE('',#2857,#718) ;
#600 = LINE('',#2862,#719) ;
#601 = LINE('',#2864,#720) ;
#602 = LINE('',#2866,#721) ;
#603 = LINE('',#2867,#722) ;
#604 = LINE('',#2870,#723) ;
#605 = LINE('',#2872,#724) ;
#606 = LINE('',#2873,#725) ;
#607 = LINE('',#2876,#726) ;
#608 = LINE('',#2878,#727) ;
#609 = LINE('',#2879,#728) ;
#610 = LINE('',#2881,#729) ;
#611 = LINE('',#2882,#730) ;
#612 = LINE('',#2890,#731) ;
#613 = LINE('',#2896,#732) ;
#614 = LINE('',#2901,#733) ;
#615 = LINE('',#2903,#734) ;
#616 = LINE('',#2905,#735) ;
#617 = LINE('',#2906,#736) ;
#618 = LINE('',#2910,#737) ;
#619 = LINE('',#2912,#738) ;
#620 = LINE('',#2914,#739) ;
#621 = LINE('',#2915,#740) ;
#622 = LINE('',#2918,#741) ;
#623 = LINE('',#2920,#742) ;
#624 = LINE('',#2921,#743) ;
#625 = LINE('',#2924,#744) ;
#626 = LINE('',#2926,#745) ;
#627 = LINE('',#2927,#746) ;
#628 = LINE('',#2930,#747) ;
#629 = LINE('',#2932,#748) ;
#630 = LINE('',#2933,#749) ;
#631 = LINE('',#2937,#750) ;
#632 = LINE('',#2938,#751) ;
#633 = LINE('',#2939,#752) ;
#634 = LINE('',#2941,#753) ;
#635 = LINE('',#2942,#754) ;
#636 = LINE('',#2946,#755) ;
#637 = LINE('',#2947,#756) ;
#638 = LINE('',#2948,#757) ;
#639 = LINE('',#2951,#758) ;
#640 = LINE('',#2953,#759) ;
#641 = LINE('',#2954,#760) ;
#642 = LINE('',#2956,#761) ;
#643 = LINE('',#2957,#762) ;
#644 = LINE('',#3000,#763) ;
#645 = LINE('',#3049,#764) ;
#646 = LINE('',#3054,#765) ;
#647 = LINE('',#3055,#766) ;
#648 = LINE('',#3058,#767) ;
#649 = LINE('',#3067,#768) ;
#650 = LINE('',#3076,#769) ;
#651 = LINE('',#3082,#770) ;
#652 = LINE('',#3087,#771) ;
#653 = LINE('',#3089,#772) ;
#654 = LINE('',#3091,#773) ;
#655 = LINE('',#3092,#774) ;
#656 = LINE('',#3095,#775) ;
#657 = LINE('',#3097,#776) ;
#658 = LINE('',#3098,#777) ;
#659 = LINE('',#3101,#778) ;
#660 = LINE('',#3103,#779) ;
#661 = LINE('',#3104,#780) ;
#662 = LINE('',#3106,#781) ;
#663 = LINE('',#3107,#782) ;
#664 = LINE('',#3116,#783) ;
#665 = LINE('',#3120,#784) ;
#666 = LINE('',#3125,#785) ;
#667 = LINE('',#3131,#786) ;
#668 = LINE('',#3137,#787) ;
#669 = LINE('',#3148,#788) ;
#670 = LINE('',#3152,#789) ;
#671 = LINE('',#3157,#790) ;
#672 = LINE('',#3163,#791) ;
#673 = LINE('',#3169,#792) ;
#674 = LINE('',#3197,#793) ;
#675 = LINE('',#3202,#794) ;
#676 = LINE('',#3205,#795) ;
#677 = LINE('',#3214,#796) ;
#678 = LINE('',#3220,#797) ;
#679 = LINE('',#3241,#798) ;
#680 = LINE('',#3250,#799) ;
#681 = LINE('',#3260,#800) ;
#682 = LINE('',#3276,#801) ;
#683 = LINE('',#3284,#802) ;
#684 = LINE('',#3290,#803) ;
#685 = LINE('',#3323,#804) ;
#686 = LINE('',#3329,#805) ;
#687 = LINE('',#3332,#806) ;
#688 = LINE('',#3337,#807) ;
#689 = LINE('',#3338,#808) ;
#690 = LINE('',#3341,#809) ;
#691 = LINE('',#3342,#810) ;
#692 = LINE('',#3345,#811) ;
#693 = LINE('',#3346,#812) ;
#694 = LINE('',#3349,#813) ;
#695 = LINE('',#3350,#814) ;
#696 = LINE('',#3353,#815) ;
#697 = LINE('',#3354,#816) ;
#698 = LINE('',#3357,#817) ;
#699 = LINE('',#3358,#818) ;
#700 = LINE('',#3421,#819) ;
#701 = LINE('',#3422,#820) ;
#702 = LINE('',#3424,#821) ;
#703 = LINE('',#3426,#822) ;
#704 = LINE('',#3428,#823) ;
#705 = LINE('',#3430,#824) ;
#706 = VECTOR('',#2222,1000.) ;
#707 = VECTOR('',#2223,1000.) ;
#708 = VECTOR('',#2224,1000.) ;
#709 = VECTOR('',#2225,1000.) ;
#710 = VECTOR('',#2228,1000.) ;
#711 = VECTOR('',#2229,1000.) ;
#712 = VECTOR('',#2230,1000.) ;
#713 = VECTOR('',#2233,1000.) ;
#714 = VECTOR('',#2234,1000.) ;
#715 = VECTOR('',#2235,1000.) ;
#716 = VECTOR('',#2238,1000.) ;
#717 = VECTOR('',#2239,1000.) ;
#718 = VECTOR('',#2250,20.) ;
#719 = VECTOR('',#2255,1000.) ;
#720 = VECTOR('',#2256,1000.) ;
#721 = VECTOR('',#2257,1000.) ;
#722 = VECTOR('',#2258,1000.) ;
#723 = VECTOR('',#2261,1000.) ;
#724 = VECTOR('',#2262,1000.) ;
#725 = VECTOR('',#2263,1000.) ;
#726 = VECTOR('',#2266,1000.) ;
#727 = VECTOR('',#2267,1000.) ;
#728 = VECTOR('',#2268,1000.) ;
#729 = VECTOR('',#2271,1000.) ;
#730 = VECTOR('',#2272,1000.) ;
#731 = VECTOR('',#2283,15.) ;
#732 = VECTOR('',#2290,15.) ;
#733 = VECTOR('',#2295,1000.) ;
#734 = VECTOR('',#2296,1000.) ;
#735 = VECTOR('',#2297,1000.) ;
#736 = VECTOR('',#2298,1000.) ;
#737 = VECTOR('',#2301,1000.) ;
#738 = VECTOR('',#2302,1000.) ;
#739 = VECTOR('',#2303,1000.) ;
#740 = VECTOR('',#2304,1000.) ;
#741 = VECTOR('',#2307,1000.) ;
#742 = VECTOR('',#2308,1000.) ;
#743 = VECTOR('',#2309,1000.) ;
#744 = VECTOR('',#2312,1000.) ;
#745 = VECTOR('',#2313,1000.) ;
#746 = VECTOR('',#2314,1000.) ;
#747 = VECTOR('',#2317,1000.) ;
#748 = VECTOR('',#2318,1000.) ;
#749 = VECTOR('',#2319,1000.) ;
#750 = VECTOR('',#2322,1000.) ;
#751 = VECTOR('',#2323,1000.) ;
#752 = VECTOR('',#2324,1000.) ;
#753 = VECTOR('',#2327,1000.) ;
#754 = VECTOR('',#2328,1000.) ;
#755 = VECTOR('',#2331,1000.) ;
#756 = VECTOR('',#2332,1000.) ;
#757 = VECTOR('',#2333,1000.) ;
#758 = VECTOR('',#2336,1000.) ;
#759 = VECTOR('',#2337,1000.) ;
#760 = VECTOR('',#2338,1000.) ;
#761 = VECTOR('',#2341,1000.) ;
#762 = VECTOR('',#2342,1000.) ;
#763 = VECTOR('',#2361,5.00000000000002) ;
#764 = VECTOR('',#2366,22.7551020408163) ;
#765 = VECTOR('',#2373,22.7551020408163) ;
#766 = VECTOR('',#2374,22.7551020408163) ;
#767 = VECTOR('',#2377,15.) ;
#768 = VECTOR('',#2390,5.) ;
#769 = VECTOR('',#2403,15.) ;
#770 = VECTOR('',#2410,15.) ;
#771 = VECTOR('',#2415,1000.) ;
#772 = VECTOR('',#2416,1000.) ;
#773 = VECTOR('',#2417,1000.) ;
#774 = VECTOR('',#2418,1000.) ;
#775 = VECTOR('',#2421,1000.) ;
#776 = VECTOR('',#2422,1000.) ;
#777 = VECTOR('',#2423,1000.) ;
#778 = VECTOR('',#2426,1000.) ;
#779 = VECTOR('',#2427,1000.) ;
#780 = VECTOR('',#2428,1000.) ;
#781 = VECTOR('',#2431,1000.) ;
#782 = VECTOR('',#2432,1000.) ;
#783 = VECTOR('',#2445,3.39999999999999) ;
#784 = VECTOR('',#2450,3.39999999999999) ;
#785 = VECTOR('',#2455,12.5) ;
#786 = VECTOR('',#2462,15.) ;
#787 = VECTOR('',#2469,17.5) ;
#788 = VECTOR('',#2486,3.39999999999999) ;
#789 = VECTOR('',#2491,3.39999999999999) ;
#790 = VECTOR('',#2496,12.5) ;
#791 = VECTOR('',#2503,15.) ;
#792 = VECTOR('',#2510,17.5) ;
#793 = VECTOR('',#2553,12.5) ;
#794 = VECTOR('',#2560,50.) ;
#795 = VECTOR('',#2563,50.) ;
#796 = VECTOR('',#2576,4.5) ;
#797 = VECTOR('',#2583,25.) ;
#798 = VECTOR('',#2618,27.5) ;
#799 = VECTOR('',#2629,23.75) ;
#800 = VECTOR('',#2640,23.75) ;
#801 = VECTOR('',#2661,15.) ;
#802 = VECTOR('',#2672,18.75) ;
#803 = VECTOR('',#2679,18.75) ;
#804 = VECTOR('',#2722,6.5) ;
#805 = VECTOR('',#2729,3.3095) ;
#806 = VECTOR('',#2734,4.) ;
#807 = VECTOR('',#2741,1000.) ;
#808 = VECTOR('',#2742,1000.) ;
#809 = VECTOR('',#2745,1000.) ;
#810 = VECTOR('',#2746,1000.) ;
#811 = VECTOR('',#2749,1000.) ;
#812 = VECTOR('',#2750,1000.) ;
#813 = VECTOR('',#2753,1000.) ;
#814 = VECTOR('',#2754,1000.) ;
#815 = VECTOR('',#2757,1000.) ;
#816 = VECTOR('',#2758,1000.) ;
#817 = VECTOR('',#2761,1000.) ;
#818 = VECTOR('',#2762,1000.) ;
#819 = VECTOR('',#2791,1000.) ;
#820 = VECTOR('',#2792,1000.) ;
#821 = VECTOR('',#2795,1000.) ;
#822 = VECTOR('',#2798,1000.) ;
#823 = VECTOR('',#2801,1000.) ;
#824 = VECTOR('',#2804,1000.) ;
#825 = VERTEX_POINT('',#2827) ;
#826 = VERTEX_POINT('',#2828) ;
#827 = VERTEX_POINT('',#2830) ;
#828 = VERTEX_POINT('',#2832) ;
#829 = VERTEX_POINT('',#2836) ;
#830 = VERTEX_POINT('',#2838) ;
#831 = VERTEX_POINT('',#2842) ;
#832 = VERTEX_POINT('',#2844) ;
#833 = VERTEX_POINT('',#2854) ;
#834 = VERTEX_POINT('',#2856) ;
#835 = VERTEX_POINT('',#2860) ;
#836 = VERTEX_POINT('',#2861) ;
#837 = VERTEX_POINT('',#2863) ;
#838 = VERTEX_POINT('',#2865) ;
#839 = VERTEX_POINT('',#2869) ;
#840 = VERTEX_POINT('',#2871) ;
#841 = VERTEX_POINT('',#2875) ;
#842 = VERTEX_POINT('',#2877) ;
#843 = VERTEX_POINT('',#2887) ;
#844 = VERTEX_POINT('',#2889) ;
#845 = VERTEX_POINT('',#2893) ;
#846 = VERTEX_POINT('',#2895) ;
#847 = VERTEX_POINT('',#2899) ;
#848 = VERTEX_POINT('',#2900) ;
#849 = VERTEX_POINT('',#2902) ;
#850 = VERTEX_POINT('',#2904) ;
#851 = VERTEX_POINT('',#2908) ;
#852 = VERTEX_POINT('',#2909) ;
#853 = VERTEX_POINT('',#2911) ;
#854 = VERTEX_POINT('',#2913) ;
#855 = VERTEX_POINT('',#2917) ;
#856 = VERTEX_POINT('',#2919) ;
#857 = VERTEX_POINT('',#2923) ;
#858 = VERTEX_POINT('',#2925) ;
#859 = VERTEX_POINT('',#2929) ;
#860 = VERTEX_POINT('',#2931) ;
#861 = VERTEX_POINT('',#2935) ;
#862 = VERTEX_POINT('',#2936) ;
#863 = VERTEX_POINT('',#2944) ;
#864 = VERTEX_POINT('',#2945) ;
#865 = VERTEX_POINT('',#2950) ;
#866 = VERTEX_POINT('',#2952) ;
#867 = VERTEX_POINT('',#2967) ;
#868 = VERTEX_POINT('',#2968) ;
#869 = VERTEX_POINT('',#2988) ;
#870 = VERTEX_POINT('',#2999) ;
#871 = VERTEX_POINT('',#3046) ;
#872 = VERTEX_POINT('',#3048) ;
#873 = VERTEX_POINT('',#3052) ;
#874 = VERTEX_POINT('',#3057) ;
#875 = VERTEX_POINT('',#3064) ;
#876 = VERTEX_POINT('',#3066) ;
#877 = VERTEX_POINT('',#3073) ;
#878 = VERTEX_POINT('',#3075) ;
#879 = VERTEX_POINT('',#3079) ;
#880 = VERTEX_POINT('',#3081) ;
#881 = VERTEX_POINT('',#3085) ;
#882 = VERTEX_POINT('',#3086) ;
#883 = VERTEX_POINT('',#3088) ;
#884 = VERTEX_POINT('',#3090) ;
#885 = VERTEX_POINT('',#3094) ;
#886 = VERTEX_POINT('',#3096) ;
#887 = VERTEX_POINT('',#3100) ;
#888 = VERTEX_POINT('',#3102) ;
#889 = VERTEX_POINT('',#3113) ;
#890 = VERTEX_POINT('',#3115) ;
#891 = VERTEX_POINT('',#3119) ;
#892 = VERTEX_POINT('',#3122) ;
#893 = VERTEX_POINT('',#3124) ;
#894 = VERTEX_POINT('',#3128) ;
#895 = VERTEX_POINT('',#3130) ;
#896 = VERTEX_POINT('',#3134) ;
#897 = VERTEX_POINT('',#3136) ;
#898 = VERTEX_POINT('',#3145) ;
#899 = VERTEX_POINT('',#3147) ;
#900 = VERTEX_POINT('',#3151) ;
#901 = VERTEX_POINT('',#3154) ;
#902 = VERTEX_POINT('',#3156) ;
#903 = VERTEX_POINT('',#3160) ;
#904 = VERTEX_POINT('',#3162) ;
#905 = VERTEX_POINT('',#3166) ;
#906 = VERTEX_POINT('',#3168) ;
#907 = VERTEX_POINT('',#3184) ;
#908 = VERTEX_POINT('',#3185) ;
#909 = VERTEX_POINT('',#3187) ;
#910 = VERTEX_POINT('',#3189) ;
#911 = VERTEX_POINT('',#3194) ;
#912 = VERTEX_POINT('',#3196) ;
#913 = VERTEX_POINT('',#3200) ;
#914 = VERTEX_POINT('',#3204) ;
#915 = VERTEX_POINT('',#3211) ;
#916 = VERTEX_POINT('',#3213) ;
#917 = VERTEX_POINT('',#3217) ;
#918 = VERTEX_POINT('',#3219) ;
#919 = VERTEX_POINT('',#3233) ;
#920 = VERTEX_POINT('',#3235) ;
#921 = VERTEX_POINT('',#3239) ;
#922 = VERTEX_POINT('',#3243) ;
#923 = VERTEX_POINT('',#3247) ;
#924 = VERTEX_POINT('',#3249) ;
#925 = VERTEX_POINT('',#3251) ;
#926 = VERTEX_POINT('',#3255) ;
#927 = VERTEX_POINT('',#3256) ;
#928 = VERTEX_POINT('',#3259) ;
#929 = VERTEX_POINT('',#3263) ;
#930 = VERTEX_POINT('',#3264) ;
#931 = VERTEX_POINT('',#3269) ;
#932 = VERTEX_POINT('',#3271) ;
#933 = VERTEX_POINT('',#3275) ;
#934 = VERTEX_POINT('',#3279) ;
#935 = VERTEX_POINT('',#3283) ;
#936 = VERTEX_POINT('',#3287) ;
#937 = VERTEX_POINT('',#3289) ;
#938 = VERTEX_POINT('',#3291) ;
#939 = VERTEX_POINT('',#3302) ;
#940 = VERTEX_POINT('',#3303) ;
#941 = VERTEX_POINT('',#3306) ;
#942 = VERTEX_POINT('',#3310) ;
#943 = VERTEX_POINT('',#3311) ;
#944 = VERTEX_POINT('',#3313) ;
#945 = VERTEX_POINT('',#3315) ;
#946 = VERTEX_POINT('',#3317) ;
#947 = VERTEX_POINT('',#3319) ;
#948 = VERTEX_POINT('',#3322) ;
#949 = VERTEX_POINT('',#3326) ;
#950 = VERTEX_POINT('',#3328) ;
#951 = VERTEX_POINT('',#3336) ;
#952 = VERTEX_POINT('',#3340) ;
#953 = VERTEX_POINT('',#3344) ;
#954 = VERTEX_POINT('',#3348) ;
#955 = VERTEX_POINT('',#3352) ;
#956 = VERTEX_POINT('',#3356) ;
#957 = VERTEX_POINT('',#3360) ;
#958 = VERTEX_POINT('',#3361) ;
#959 = VERTEX_POINT('',#3363) ;
#960 = VERTEX_POINT('',#3365) ;
#961 = VERTEX_POINT('',#3367) ;
#962 = VERTEX_POINT('',#3369) ;
#963 = VERTEX_POINT('',#3373) ;
#964 = VERTEX_POINT('',#3381) ;
#965 = VERTEX_POINT('',#3389) ;
#966 = VERTEX_POINT('',#3397) ;
#967 = VERTEX_POINT('',#3405) ;
#968 = VERTEX_POINT('',#3413) ;
#969 = EDGE_CURVE('',#825,#826,#587,.T.) ;
#970 = EDGE_CURVE('',#827,#825,#588,.T.) ;
#971 = EDGE_CURVE('',#827,#828,#589,.T.) ;
#972 = EDGE_CURVE('',#828,#826,#590,.T.) ;
#973 = EDGE_CURVE('',#829,#825,#591,.T.) ;
#974 = EDGE_CURVE('',#830,#829,#592,.T.) ;
#975 = EDGE_CURVE('',#830,#827,#593,.T.) ;
#976 = EDGE_CURVE('',#831,#829,#594,.T.) ;
#977 = EDGE_CURVE('',#832,#831,#595,.T.) ;
#978 = EDGE_CURVE('',#832,#830,#596,.T.) ;
#979 = EDGE_CURVE('',#826,#831,#597,.T.) ;
#980 = EDGE_CURVE('',#828,#832,#598,.T.) ;
#981 = EDGE_CURVE('',#833,#833,#166,.T.) ;
#982 = EDGE_CURVE('',#833,#834,#599,.T.) ;
#983 = EDGE_CURVE('',#834,#834,#167,.T.) ;
#984 = EDGE_CURVE('',#835,#836,#600,.T.) ;
#985 = EDGE_CURVE('',#837,#835,#601,.T.) ;
#986 = EDGE_CURVE('',#837,#838,#602,.T.) ;
#987 = EDGE_CURVE('',#838,#836,#603,.T.) ;
#988 = EDGE_CURVE('',#839,#835,#604,.T.) ;
#989 = EDGE_CURVE('',#840,#839,#605,.T.) ;
#990 = EDGE_CURVE('',#840,#837,#606,.T.) ;
#991 = EDGE_CURVE('',#841,#839,#607,.T.) ;
#992 = EDGE_CURVE('',#842,#841,#608,.T.) ;
#993 = EDGE_CURVE('',#842,#840,#609,.T.) ;
#994 = EDGE_CURVE('',#836,#841,#610,.T.) ;
#995 = EDGE_CURVE('',#838,#842,#611,.T.) ;
#996 = EDGE_CURVE('',#843,#843,#168,.T.) ;
#997 = EDGE_CURVE('',#843,#844,#612,.T.) ;
#998 = EDGE_CURVE('',#844,#844,#169,.T.) ;
#999 = EDGE_CURVE('',#845,#845,#170,.T.) ;
#1000 = EDGE_CURVE('',#845,#846,#613,.T.) ;
#1001 = EDGE_CURVE('',#846,#846,#171,.T.) ;
#1002 = EDGE_CURVE('',#847,#848,#614,.T.) ;
#1003 = EDGE_CURVE('',#849,#847,#615,.T.) ;
#1004 = EDGE_CURVE('',#850,#849,#616,.T.) ;
#1005 = EDGE_CURVE('',#850,#848,#617,.T.) ;
#1006 = EDGE_CURVE('',#851,#852,#618,.T.) ;
#1007 = EDGE_CURVE('',#853,#851,#619,.T.) ;
#1008 = EDGE_CURVE('',#853,#854,#620,.T.) ;
#1009 = EDGE_CURVE('',#854,#852,#621,.T.) ;
#1010 = EDGE_CURVE('',#855,#851,#622,.T.) ;
#1011 = EDGE_CURVE('',#856,#855,#623,.T.) ;
#1012 = EDGE_CURVE('',#856,#853,#624,.T.) ;
#1013 = EDGE_CURVE('',#857,#855,#625,.T.) ;
#1014 = EDGE_CURVE('',#858,#857,#626,.T.) ;
#1015 = EDGE_CURVE('',#858,#856,#627,.T.) ;
#1016 = EDGE_CURVE('',#859,#857,#628,.T.) ;
#1017 = EDGE_CURVE('',#860,#859,#629,.T.) ;
#1018 = EDGE_CURVE('',#860,#858,#630,.T.) ;
#1019 = EDGE_CURVE('',#861,#862,#631,.T.) ;
#1020 = EDGE_CURVE('',#861,#860,#632,.T.) ;
#1021 = EDGE_CURVE('',#862,#859,#633,.T.) ;
#1022 = EDGE_CURVE('',#852,#849,#634,.T.) ;
#1023 = EDGE_CURVE('',#854,#850,#635,.T.) ;
#1024 = EDGE_CURVE('',#863,#864,#636,.T.) ;
#1025 = EDGE_CURVE('',#864,#848,#637,.T.) ;
#1026 = EDGE_CURVE('',#861,#863,#638,.T.) ;
#1027 = EDGE_CURVE('',#865,#847,#639,.T.) ;
#1028 = EDGE_CURVE('',#866,#865,#640,.T.) ;
#1029 = EDGE_CURVE('',#862,#866,#641,.T.) ;
#1030 = EDGE_CURVE('',#863,#866,#642,.T.) ;
#1031 = EDGE_CURVE('',#864,#865,#643,.T.) ;
#1032 = EDGE_CURVE('',#867,#868,#41,.T.) ;
#1033 = EDGE_CURVE('',#868,#869,#42,.T.) ;
#1034 = EDGE_CURVE('',#869,#870,#644,.T.) ;
#1035 = EDGE_CURVE('',#870,#870,#43,.T.) ;
#1036 = EDGE_CURVE('',#869,#867,#44,.T.) ;
#1037 = EDGE_CURVE('',#871,#871,#172,.T.) ;
#1038 = EDGE_CURVE('',#871,#872,#645,.T.) ;
#1039 = EDGE_CURVE('',#872,#872,#173,.T.) ;
#1040 = EDGE_CURVE('',#873,#873,#174,.T.) ;
#1041 = EDGE_CURVE('',#873,#867,#646,.T.) ;
#1042 = EDGE_CURVE('',#868,#871,#647,.T.) ;
#1043 = EDGE_CURVE('',#872,#874,#648,.T.) ;
#1044 = EDGE_CURVE('',#874,#874,#175,.T.) ;
#1045 = EDGE_CURVE('',#875,#875,#176,.T.) ;
#1046 = EDGE_CURVE('',#875,#876,#649,.T.) ;
#1047 = EDGE_CURVE('',#876,#876,#177,.T.) ;
#1048 = EDGE_CURVE('',#877,#877,#178,.T.) ;
#1049 = EDGE_CURVE('',#877,#878,#650,.T.) ;
#1050 = EDGE_CURVE('',#878,#878,#179,.T.) ;
#1051 = EDGE_CURVE('',#879,#879,#180,.T.) ;
#1052 = EDGE_CURVE('',#879,#880,#651,.T.) ;
#1053 = EDGE_CURVE('',#880,#880,#181,.T.) ;
#1054 = EDGE_CURVE('',#881,#882,#652,.T.) ;
#1055 = EDGE_CURVE('',#883,#882,#653,.T.) ;
#1056 = EDGE_CURVE('',#884,#883,#654,.T.) ;
#1057 = EDGE_CURVE('',#884,#881,#655,.T.) ;
#1058 = EDGE_CURVE('',#882,#885,#656,.T.) ;
#1059 = EDGE_CURVE('',#886,#885,#657,.T.) ;
#1060 = EDGE_CURVE('',#883,#886,#658,.T.) ;
#1061 = EDGE_CURVE('',#885,#887,#659,.T.) ;
#1062 = EDGE_CURVE('',#888,#887,#660,.T.) ;
#1063 = EDGE_CURVE('',#886,#888,#661,.T.) ;
#1064 = EDGE_CURVE('',#887,#881,#662,.T.) ;
#1065 = EDGE_CURVE('',#888,#884,#663,.T.) ;
#1066 = EDGE_CURVE('',#889,#889,#182,.T.) ;
#1067 = EDGE_CURVE('',#889,#890,#664,.T.) ;
#1068 = EDGE_CURVE('',#890,#890,#183,.T.) ;
#1069 = EDGE_CURVE('',#891,#889,#665,.T.) ;
#1070 = EDGE_CURVE('',#892,#892,#184,.T.) ;
#1071 = EDGE_CURVE('',#892,#893,#666,.T.) ;
#1072 = EDGE_CURVE('',#893,#893,#185,.T.) ;
#1073 = EDGE_CURVE('',#894,#894,#186,.T.) ;
#1074 = EDGE_CURVE('',#894,#895,#667,.T.) ;
#1075 = EDGE_CURVE('',#895,#895,#187,.T.) ;
#1076 = EDGE_CURVE('',#896,#896,#188,.T.) ;
#1077 = EDGE_CURVE('',#896,#897,#668,.T.) ;
#1078 = EDGE_CURVE('',#897,#897,#189,.T.) ;
#1079 = EDGE_CURVE('',#898,#898,#190,.T.) ;
#1080 = EDGE_CURVE('',#898,#899,#669,.T.) ;
#1081 = EDGE_CURVE('',#899,#899,#191,.T.) ;
#1082 = EDGE_CURVE('',#900,#898,#670,.T.) ;
#1083 = EDGE_CURVE('',#901,#901,#192,.T.) ;
#1084 = EDGE_CURVE('',#901,#902,#671,.T.) ;
#1085 = EDGE_CURVE('',#902,#902,#193,.T.) ;
#1086 = EDGE_CURVE('',#903,#903,#194,.T.) ;
#1087 = EDGE_CURVE('',#903,#904,#672,.T.) ;
#1088 = EDGE_CURVE('',#904,#904,#195,.T.) ;
#1089 = EDGE_CURVE('',#905,#905,#196,.T.) ;
#1090 = EDGE_CURVE('',#905,#906,#673,.T.) ;
#1091 = EDGE_CURVE('',#906,#906,#197,.T.) ;
#1092 = EDGE_CURVE('',#907,#908,#198,.T.) ;
#1093 = EDGE_CURVE('',#908,#909,#199,.T.) ;
#1094 = EDGE_CURVE('',#909,#910,#200,.T.) ;
#1095 = EDGE_CURVE('',#910,#909,#201,.T.) ;
#1096 = EDGE_CURVE('',#908,#907,#202,.T.) ;
#1097 = EDGE_CURVE('',#911,#911,#203,.T.) ;
#1098 = EDGE_CURVE('',#911,#912,#674,.T.) ;
#1099 = EDGE_CURVE('',#912,#912,#204,.T.) ;
#1100 = EDGE_CURVE('',#913,#913,#205,.T.) ;
#1101 = EDGE_CURVE('',#913,#910,#675,.T.) ;
#1102 = EDGE_CURVE('',#907,#914,#676,.T.) ;
#1103 = EDGE_CURVE('',#914,#914,#206,.T.) ;
#1104 = EDGE_CURVE('',#915,#915,#207,.T.) ;
#1105 = EDGE_CURVE('',#915,#916,#677,.T.) ;
#1106 = EDGE_CURVE('',#916,#916,#208,.T.) ;
#1107 = EDGE_CURVE('',#917,#917,#209,.T.) ;
#1108 = EDGE_CURVE('',#917,#918,#678,.T.) ;
#1109 = EDGE_CURVE('',#918,#918,#210,.T.) ;
#1110 = EDGE_CURVE('',#919,#919,#211,.T.) ;
#1111 = EDGE_CURVE('',#919,#920,#212,.T.) ;
#1112 = EDGE_CURVE('',#920,#920,#213,.T.) ;
#1113 = EDGE_CURVE('',#921,#921,#214,.T.) ;
#1114 = EDGE_CURVE('',#921,#919,#679,.T.) ;
#1115 = EDGE_CURVE('',#922,#922,#215,.T.) ;
#1116 = EDGE_CURVE('',#922,#921,#216,.T.) ;
#1117 = EDGE_CURVE('',#923,#923,#217,.T.) ;
#1118 = EDGE_CURVE('',#923,#924,#680,.T.) ;
#1119 = EDGE_CURVE('',#925,#924,#218,.T.) ;
#1120 = EDGE_CURVE('',#924,#925,#219,.T.) ;
#1121 = EDGE_CURVE('',#926,#927,#220,.T.) ;
#1122 = EDGE_CURVE('',#927,#926,#221,.T.) ;
#1123 = EDGE_CURVE('',#927,#928,#681,.T.) ;
#1124 = EDGE_CURVE('',#928,#928,#222,.T.) ;
#1125 = EDGE_CURVE('',#929,#930,#223,.T.) ;
#1126 = EDGE_CURVE('',#930,#925,#224,.T.) ;
#1127 = EDGE_CURVE('',#930,#929,#225,.T.) ;
#1128 = EDGE_CURVE('',#931,#931,#226,.T.) ;
#1129 = EDGE_CURVE('',#931,#932,#227,.T.) ;
#1130 = EDGE_CURVE('',#932,#932,#228,.T.) ;
#1131 = EDGE_CURVE('',#932,#933,#682,.T.) ;
#1132 = EDGE_CURVE('',#933,#933,#229,.T.) ;
#1133 = EDGE_CURVE('',#933,#934,#230,.T.) ;
#1134 = EDGE_CURVE('',#934,#934,#231,.T.) ;
#1135 = EDGE_CURVE('',#929,#935,#683,.T.) ;
#1136 = EDGE_CURVE('',#935,#935,#232,.T.) ;
#1137 = EDGE_CURVE('',#936,#936,#233,.T.) ;
#1138 = EDGE_CURVE('',#936,#937,#684,.T.) ;
#1139 = EDGE_CURVE('',#938,#937,#234,.T.) ;
#1140 = EDGE_CURVE('',#937,#938,#235,.T.) ;
#1141 = EDGE_CURVE('',#926,#938,#236,.T.) ;
#1142 = EDGE_CURVE('',#939,#940,#237,.T.) ;
#1143 = EDGE_CURVE('',#940,#939,#238,.T.) ;
#1144 = EDGE_CURVE('',#940,#941,#239,.T.) ;
#1145 = EDGE_CURVE('',#941,#941,#240,.T.) ;
#1146 = EDGE_CURVE('',#942,#943,#241,.T.) ;
#1147 = EDGE_CURVE('',#944,#942,#242,.T.) ;
#1148 = EDGE_CURVE('',#945,#944,#243,.T.) ;
#1149 = EDGE_CURVE('',#946,#945,#244,.T.) ;
#1150 = EDGE_CURVE('',#947,#946,#245,.T.) ;
#1151 = EDGE_CURVE('',#943,#947,#246,.T.) ;
#1152 = EDGE_CURVE('',#943,#948,#685,.T.) ;
#1153 = EDGE_CURVE('',#948,#948,#247,.T.) ;
#1154 = EDGE_CURVE('',#949,#949,#248,.T.) ;
#1155 = EDGE_CURVE('',#949,#950,#686,.T.) ;
#1156 = EDGE_CURVE('',#950,#950,#249,.T.) ;
#1157 = EDGE_CURVE('',#939,#949,#687,.T.) ;
#1158 = EDGE_CURVE('',#951,#942,#688,.T.) ;
#1159 = EDGE_CURVE('',#943,#951,#689,.T.) ;
#1160 = EDGE_CURVE('',#942,#952,#690,.T.) ;
#1161 = EDGE_CURVE('',#952,#944,#691,.T.) ;
#1162 = EDGE_CURVE('',#944,#953,#692,.T.) ;
#1163 = EDGE_CURVE('',#953,#945,#693,.T.) ;
#1164 = EDGE_CURVE('',#945,#954,#694,.T.) ;
#1165 = EDGE_CURVE('',#954,#946,#695,.T.) ;
#1166 = EDGE_CURVE('',#946,#955,#696,.T.) ;
#1167 = EDGE_CURVE('',#955,#947,#697,.T.) ;
#1168 = EDGE_CURVE('',#947,#956,#698,.T.) ;
#1169 = EDGE_CURVE('',#956,#943,#699,.T.) ;
#1170 = EDGE_CURVE('',#957,#958,#250,.T.) ;
#1171 = EDGE_CURVE('',#959,#957,#251,.T.) ;
#1172 = EDGE_CURVE('',#960,#959,#252,.T.) ;
#1173 = EDGE_CURVE('',#961,#960,#253,.T.) ;
#1174 = EDGE_CURVE('',#961,#962,#254,.T.) ;
#1175 = EDGE_CURVE('',#958,#962,#255,.T.) ;
#1176 = EDGE_CURVE('',#962,#963,#11,.T.) ;
#1177 = EDGE_CURVE('',#963,#958,#12,.T.) ;
#1178 = EDGE_CURVE('',#961,#964,#13,.T.) ;
#1179 = EDGE_CURVE('',#964,#962,#14,.T.) ;
#1180 = EDGE_CURVE('',#965,#961,#15,.T.) ;
#1181 = EDGE_CURVE('',#960,#965,#16,.T.) ;
#1182 = EDGE_CURVE('',#966,#960,#17,.T.) ;
#1183 = EDGE_CURVE('',#959,#966,#18,.T.) ;
#1184 = EDGE_CURVE('',#958,#967,#19,.T.) ;
#1185 = EDGE_CURVE('',#967,#957,#20,.T.) ;
#1186 = EDGE_CURVE('',#968,#959,#21,.T.) ;
#1187 = EDGE_CURVE('',#957,#968,#22,.T.) ;
#1188 = EDGE_CURVE('',#956,#968,#700,.T.) ;
#1189 = EDGE_CURVE('',#951,#967,#701,.T.) ;
#1190 = EDGE_CURVE('',#955,#966,#702,.T.) ;
#1191 = EDGE_CURVE('',#954,#965,#703,.T.) ;
#1192 = EDGE_CURVE('',#953,#964,#704,.T.) ;
#1193 = EDGE_CURVE('',#952,#963,#705,.T.) ;
#1194 = ORIENTED_EDGE('',*,*,#969,.F.) ;
#1195 = ORIENTED_EDGE('',*,*,#970,.F.) ;
#1196 = ORIENTED_EDGE('',*,*,#971,.T.) ;
#1197 = ORIENTED_EDGE('',*,*,#972,.T.) ;
#1198 = ORIENTED_EDGE('',*,*,#973,.F.) ;
#1199 = ORIENTED_EDGE('',*,*,#974,.F.) ;
#1200 = ORIENTED_EDGE('',*,*,#975,.T.) ;
#1201 = ORIENTED_EDGE('',*,*,#970,.T.) ;
#1202 = ORIENTED_EDGE('',*,*,#976,.F.) ;
#1203 = ORIENTED_EDGE('',*,*,#977,.F.) ;
#1204 = ORIENTED_EDGE('',*,*,#978,.T.) ;
#1205 = ORIENTED_EDGE('',*,*,#974,.T.) ;
#1206 = ORIENTED_EDGE('',*,*,#979,.F.) ;
#1207 = ORIENTED_EDGE('',*,*,#972,.F.) ;
#1208 = ORIENTED_EDGE('',*,*,#980,.T.) ;
#1209 = ORIENTED_EDGE('',*,*,#977,.T.) ;
#1210 = ORIENTED_EDGE('',*,*,#971,.F.) ;
#1211 = ORIENTED_EDGE('',*,*,#975,.F.) ;
#1212 = ORIENTED_EDGE('',*,*,#978,.F.) ;
#1213 = ORIENTED_EDGE('',*,*,#980,.F.) ;
#1214 = ORIENTED_EDGE('',*,*,#969,.T.) ;
#1215 = ORIENTED_EDGE('',*,*,#979,.T.) ;
#1216 = ORIENTED_EDGE('',*,*,#976,.T.) ;
#1217 = ORIENTED_EDGE('',*,*,#973,.T.) ;
#1218 = ORIENTED_EDGE('',*,*,#981,.F.) ;
#1219 = ORIENTED_EDGE('',*,*,#982,.T.) ;
#1220 = ORIENTED_EDGE('',*,*,#983,.T.) ;
#1221 = ORIENTED_EDGE('',*,*,#982,.F.) ;
#1222 = ORIENTED_EDGE('',*,*,#984,.F.) ;
#1223 = ORIENTED_EDGE('',*,*,#985,.F.) ;
#1224 = ORIENTED_EDGE('',*,*,#986,.T.) ;
#1225 = ORIENTED_EDGE('',*,*,#987,.T.) ;
#1226 = ORIENTED_EDGE('',*,*,#988,.F.) ;
#1227 = ORIENTED_EDGE('',*,*,#989,.F.) ;
#1228 = ORIENTED_EDGE('',*,*,#990,.T.) ;
#1229 = ORIENTED_EDGE('',*,*,#985,.T.) ;
#1230 = ORIENTED_EDGE('',*,*,#991,.F.) ;
#1231 = ORIENTED_EDGE('',*,*,#992,.F.) ;
#1232 = ORIENTED_EDGE('',*,*,#993,.T.) ;
#1233 = ORIENTED_EDGE('',*,*,#989,.T.) ;
#1234 = ORIENTED_EDGE('',*,*,#994,.F.) ;
#1235 = ORIENTED_EDGE('',*,*,#987,.F.) ;
#1236 = ORIENTED_EDGE('',*,*,#995,.T.) ;
#1237 = ORIENTED_EDGE('',*,*,#992,.T.) ;
#1238 = ORIENTED_EDGE('',*,*,#986,.F.) ;
#1239 = ORIENTED_EDGE('',*,*,#990,.F.) ;
#1240 = ORIENTED_EDGE('',*,*,#993,.F.) ;
#1241 = ORIENTED_EDGE('',*,*,#995,.F.) ;
#1242 = ORIENTED_EDGE('',*,*,#983,.F.) ;
#1243 = ORIENTED_EDGE('',*,*,#984,.T.) ;
#1244 = ORIENTED_EDGE('',*,*,#994,.T.) ;
#1245 = ORIENTED_EDGE('',*,*,#991,.T.) ;
#1246 = ORIENTED_EDGE('',*,*,#988,.T.) ;
#1247 = ORIENTED_EDGE('',*,*,#981,.T.) ;
#1248 = ORIENTED_EDGE('',*,*,#996,.F.) ;
#1249 = ORIENTED_EDGE('',*,*,#997,.T.) ;
#1250 = ORIENTED_EDGE('',*,*,#998,.T.) ;
#1251 = ORIENTED_EDGE('',*,*,#997,.F.) ;
#1252 = ORIENTED_EDGE('',*,*,#999,.F.) ;
#1253 = ORIENTED_EDGE('',*,*,#1000,.T.) ;
#1254 = ORIENTED_EDGE('',*,*,#1001,.T.) ;
#1255 = ORIENTED_EDGE('',*,*,#1000,.F.) ;
#1256 = ORIENTED_EDGE('',*,*,#1002,.F.) ;
#1257 = ORIENTED_EDGE('',*,*,#1003,.F.) ;
#1258 = ORIENTED_EDGE('',*,*,#1004,.F.) ;
#1259 = ORIENTED_EDGE('',*,*,#1005,.T.) ;
#1260 = ORIENTED_EDGE('',*,*,#1006,.F.) ;
#1261 = ORIENTED_EDGE('',*,*,#1007,.F.) ;
#1262 = ORIENTED_EDGE('',*,*,#1008,.T.) ;
#1263 = ORIENTED_EDGE('',*,*,#1009,.T.) ;
#1264 = ORIENTED_EDGE('',*,*,#1010,.F.) ;
#1265 = ORIENTED_EDGE('',*,*,#1011,.F.) ;
#1266 = ORIENTED_EDGE('',*,*,#1012,.T.) ;
#1267 = ORIENTED_EDGE('',*,*,#1007,.T.) ;
#1268 = ORIENTED_EDGE('',*,*,#1013,.F.) ;
#1269 = ORIENTED_EDGE('',*,*,#1014,.F.) ;
#1270 = ORIENTED_EDGE('',*,*,#1015,.T.) ;
#1271 = ORIENTED_EDGE('',*,*,#1011,.T.) ;
#1272 = ORIENTED_EDGE('',*,*,#1016,.F.) ;
#1273 = ORIENTED_EDGE('',*,*,#1017,.F.) ;
#1274 = ORIENTED_EDGE('',*,*,#1018,.T.) ;
#1275 = ORIENTED_EDGE('',*,*,#1014,.T.) ;
#1276 = ORIENTED_EDGE('',*,*,#1019,.F.) ;
#1277 = ORIENTED_EDGE('',*,*,#1020,.T.) ;
#1278 = ORIENTED_EDGE('',*,*,#1017,.T.) ;
#1279 = ORIENTED_EDGE('',*,*,#1021,.F.) ;
#1280 = ORIENTED_EDGE('',*,*,#1022,.F.) ;
#1281 = ORIENTED_EDGE('',*,*,#1009,.F.) ;
#1282 = ORIENTED_EDGE('',*,*,#1023,.T.) ;
#1283 = ORIENTED_EDGE('',*,*,#1004,.T.) ;
#1284 = ORIENTED_EDGE('',*,*,#1024,.T.) ;
#1285 = ORIENTED_EDGE('',*,*,#1025,.T.) ;
#1286 = ORIENTED_EDGE('',*,*,#1005,.F.) ;
#1287 = ORIENTED_EDGE('',*,*,#1023,.F.) ;
#1288 = ORIENTED_EDGE('',*,*,#1008,.F.) ;
#1289 = ORIENTED_EDGE('',*,*,#1012,.F.) ;
#1290 = ORIENTED_EDGE('',*,*,#1015,.F.) ;
#1291 = ORIENTED_EDGE('',*,*,#1018,.F.) ;
#1292 = ORIENTED_EDGE('',*,*,#1020,.F.) ;
#1293 = ORIENTED_EDGE('',*,*,#1026,.T.) ;
#1294 = ORIENTED_EDGE('',*,*,#996,.T.) ;
#1295 = ORIENTED_EDGE('',*,*,#999,.T.) ;
#1296 = ORIENTED_EDGE('',*,*,#1027,.F.) ;
#1297 = ORIENTED_EDGE('',*,*,#1028,.F.) ;
#1298 = ORIENTED_EDGE('',*,*,#1029,.F.) ;
#1299 = ORIENTED_EDGE('',*,*,#1021,.T.) ;
#1300 = ORIENTED_EDGE('',*,*,#1016,.T.) ;
#1301 = ORIENTED_EDGE('',*,*,#1013,.T.) ;
#1302 = ORIENTED_EDGE('',*,*,#1010,.T.) ;
#1303 = ORIENTED_EDGE('',*,*,#1006,.T.) ;
#1304 = ORIENTED_EDGE('',*,*,#1022,.T.) ;
#1305 = ORIENTED_EDGE('',*,*,#1003,.T.) ;
#1306 = ORIENTED_EDGE('',*,*,#998,.F.) ;
#1307 = ORIENTED_EDGE('',*,*,#1001,.F.) ;
#1308 = ORIENTED_EDGE('',*,*,#1030,.T.) ;
#1309 = ORIENTED_EDGE('',*,*,#1028,.T.) ;
#1310 = ORIENTED_EDGE('',*,*,#1031,.F.) ;
#1311 = ORIENTED_EDGE('',*,*,#1024,.F.) ;
#1312 = ORIENTED_EDGE('',*,*,#1002,.T.) ;
#1313 = ORIENTED_EDGE('',*,*,#1025,.F.) ;
#1314 = ORIENTED_EDGE('',*,*,#1031,.T.) ;
#1315 = ORIENTED_EDGE('',*,*,#1027,.T.) ;
#1316 = ORIENTED_EDGE('',*,*,#1019,.T.) ;
#1317 = ORIENTED_EDGE('',*,*,#1029,.T.) ;
#1318 = ORIENTED_EDGE('',*,*,#1030,.F.) ;
#1319 = ORIENTED_EDGE('',*,*,#1026,.F.) ;
#1320 = ORIENTED_EDGE('',*,*,#1032,.T.) ;
#1321 = ORIENTED_EDGE('',*,*,#1033,.T.) ;
#1322 = ORIENTED_EDGE('',*,*,#1034,.T.) ;
#1323 = ORIENTED_EDGE('',*,*,#1035,.T.) ;
#1324 = ORIENTED_EDGE('',*,*,#1034,.F.) ;
#1325 = ORIENTED_EDGE('',*,*,#1036,.T.) ;
#1326 = ORIENTED_EDGE('',*,*,#1037,.F.) ;
#1327 = ORIENTED_EDGE('',*,*,#1038,.T.) ;
#1328 = ORIENTED_EDGE('',*,*,#1039,.F.) ;
#1329 = ORIENTED_EDGE('',*,*,#1038,.F.) ;
#1330 = ORIENTED_EDGE('',*,*,#1040,.F.) ;
#1331 = ORIENTED_EDGE('',*,*,#1041,.T.) ;
#1332 = ORIENTED_EDGE('',*,*,#1036,.F.) ;
#1333 = ORIENTED_EDGE('',*,*,#1033,.F.) ;
#1334 = ORIENTED_EDGE('',*,*,#1042,.T.) ;
#1335 = ORIENTED_EDGE('',*,*,#1037,.T.) ;
#1336 = ORIENTED_EDGE('',*,*,#1042,.F.) ;
#1337 = ORIENTED_EDGE('',*,*,#1032,.F.) ;
#1338 = ORIENTED_EDGE('',*,*,#1041,.F.) ;
#1339 = ORIENTED_EDGE('',*,*,#1035,.F.) ;
#1340 = ORIENTED_EDGE('',*,*,#1039,.T.) ;
#1341 = ORIENTED_EDGE('',*,*,#1043,.T.) ;
#1342 = ORIENTED_EDGE('',*,*,#1044,.T.) ;
#1343 = ORIENTED_EDGE('',*,*,#1043,.F.) ;
#1344 = ORIENTED_EDGE('',*,*,#1044,.F.) ;
#1345 = ORIENTED_EDGE('',*,*,#1040,.T.) ;
#1346 = ORIENTED_EDGE('',*,*,#1045,.T.) ;
#1347 = ORIENTED_EDGE('',*,*,#1046,.T.) ;
#1348 = ORIENTED_EDGE('',*,*,#1047,.F.) ;
#1349 = ORIENTED_EDGE('',*,*,#1046,.F.) ;
#1350 = ORIENTED_EDGE('',*,*,#1047,.T.) ;
#1351 = ORIENTED_EDGE('',*,*,#1045,.F.) ;
#1352 = ORIENTED_EDGE('',*,*,#1048,.F.) ;
#1353 = ORIENTED_EDGE('',*,*,#1049,.T.) ;
#1354 = ORIENTED_EDGE('',*,*,#1050,.T.) ;
#1355 = ORIENTED_EDGE('',*,*,#1049,.F.) ;
#1356 = ORIENTED_EDGE('',*,*,#1051,.F.) ;
#1357 = ORIENTED_EDGE('',*,*,#1052,.T.) ;
#1358 = ORIENTED_EDGE('',*,*,#1053,.T.) ;
#1359 = ORIENTED_EDGE('',*,*,#1052,.F.) ;
#1360 = ORIENTED_EDGE('',*,*,#1054,.T.) ;
#1361 = ORIENTED_EDGE('',*,*,#1055,.F.) ;
#1362 = ORIENTED_EDGE('',*,*,#1056,.F.) ;
#1363 = ORIENTED_EDGE('',*,*,#1057,.T.) ;
#1364 = ORIENTED_EDGE('',*,*,#1048,.T.) ;
#1365 = ORIENTED_EDGE('',*,*,#1058,.T.) ;
#1366 = ORIENTED_EDGE('',*,*,#1059,.F.) ;
#1367 = ORIENTED_EDGE('',*,*,#1060,.F.) ;
#1368 = ORIENTED_EDGE('',*,*,#1055,.T.) ;
#1369 = ORIENTED_EDGE('',*,*,#1061,.T.) ;
#1370 = ORIENTED_EDGE('',*,*,#1062,.F.) ;
#1371 = ORIENTED_EDGE('',*,*,#1063,.F.) ;
#1372 = ORIENTED_EDGE('',*,*,#1059,.T.) ;
#1373 = ORIENTED_EDGE('',*,*,#1050,.F.) ;
#1374 = ORIENTED_EDGE('',*,*,#1064,.T.) ;
#1375 = ORIENTED_EDGE('',*,*,#1057,.F.) ;
#1376 = ORIENTED_EDGE('',*,*,#1065,.F.) ;
#1377 = ORIENTED_EDGE('',*,*,#1062,.T.) ;
#1378 = ORIENTED_EDGE('',*,*,#1053,.F.) ;
#1379 = ORIENTED_EDGE('',*,*,#1056,.T.) ;
#1380 = ORIENTED_EDGE('',*,*,#1060,.T.) ;
#1381 = ORIENTED_EDGE('',*,*,#1063,.T.) ;
#1382 = ORIENTED_EDGE('',*,*,#1065,.T.) ;
#1383 = ORIENTED_EDGE('',*,*,#1054,.F.) ;
#1384 = ORIENTED_EDGE('',*,*,#1064,.F.) ;
#1385 = ORIENTED_EDGE('',*,*,#1061,.F.) ;
#1386 = ORIENTED_EDGE('',*,*,#1058,.F.) ;
#1387 = ORIENTED_EDGE('',*,*,#1051,.T.) ;
#1388 = ORIENTED_EDGE('',*,*,#1066,.F.) ;
#1389 = ORIENTED_EDGE('',*,*,#1067,.T.) ;
#1390 = ORIENTED_EDGE('',*,*,#1068,.T.) ;
#1391 = ORIENTED_EDGE('',*,*,#1067,.F.) ;
#1392 = ORIENTED_EDGE('',*,*,#1069,.T.) ;
#1393 = ORIENTED_EDGE('',*,*,#1066,.T.) ;
#1394 = ORIENTED_EDGE('',*,*,#1069,.F.) ;
#1395 = ORIENTED_EDGE('',*,*,#1070,.F.) ;
#1396 = ORIENTED_EDGE('',*,*,#1071,.T.) ;
#1397 = ORIENTED_EDGE('',*,*,#1072,.T.) ;
#1398 = ORIENTED_EDGE('',*,*,#1071,.F.) ;
#1399 = ORIENTED_EDGE('',*,*,#1073,.F.) ;
#1400 = ORIENTED_EDGE('',*,*,#1074,.T.) ;
#1401 = ORIENTED_EDGE('',*,*,#1075,.T.) ;
#1402 = ORIENTED_EDGE('',*,*,#1074,.F.) ;
#1403 = ORIENTED_EDGE('',*,*,#1076,.F.) ;
#1404 = ORIENTED_EDGE('',*,*,#1077,.T.) ;
#1405 = ORIENTED_EDGE('',*,*,#1078,.T.) ;
#1406 = ORIENTED_EDGE('',*,*,#1077,.F.) ;
#1407 = ORIENTED_EDGE('',*,*,#1078,.F.) ;
#1408 = ORIENTED_EDGE('',*,*,#1076,.T.) ;
#1409 = ORIENTED_EDGE('',*,*,#1075,.F.) ;
#1410 = ORIENTED_EDGE('',*,*,#1073,.T.) ;
#1411 = ORIENTED_EDGE('',*,*,#1072,.F.) ;
#1412 = ORIENTED_EDGE('',*,*,#1070,.T.) ;
#1413 = ORIENTED_EDGE('',*,*,#1068,.F.) ;
#1414 = ORIENTED_EDGE('',*,*,#1079,.F.) ;
#1415 = ORIENTED_EDGE('',*,*,#1080,.T.) ;
#1416 = ORIENTED_EDGE('',*,*,#1081,.T.) ;
#1417 = ORIENTED_EDGE('',*,*,#1080,.F.) ;
#1418 = ORIENTED_EDGE('',*,*,#1082,.T.) ;
#1419 = ORIENTED_EDGE('',*,*,#1079,.T.) ;
#1420 = ORIENTED_EDGE('',*,*,#1082,.F.) ;
#1421 = ORIENTED_EDGE('',*,*,#1083,.F.) ;
#1422 = ORIENTED_EDGE('',*,*,#1084,.T.) ;
#1423 = ORIENTED_EDGE('',*,*,#1085,.T.) ;
#1424 = ORIENTED_EDGE('',*,*,#1084,.F.) ;
#1425 = ORIENTED_EDGE('',*,*,#1086,.F.) ;
#1426 = ORIENTED_EDGE('',*,*,#1087,.T.) ;
#1427 = ORIENTED_EDGE('',*,*,#1088,.T.) ;
#1428 = ORIENTED_EDGE('',*,*,#1087,.F.) ;
#1429 = ORIENTED_EDGE('',*,*,#1089,.F.) ;
#1430 = ORIENTED_EDGE('',*,*,#1090,.T.) ;
#1431 = ORIENTED_EDGE('',*,*,#1091,.T.) ;
#1432 = ORIENTED_EDGE('',*,*,#1090,.F.) ;
#1433 = ORIENTED_EDGE('',*,*,#1091,.F.) ;
#1434 = ORIENTED_EDGE('',*,*,#1089,.T.) ;
#1435 = ORIENTED_EDGE('',*,*,#1088,.F.) ;
#1436 = ORIENTED_EDGE('',*,*,#1086,.T.) ;
#1437 = ORIENTED_EDGE('',*,*,#1085,.F.) ;
#1438 = ORIENTED_EDGE('',*,*,#1083,.T.) ;
#1439 = ORIENTED_EDGE('',*,*,#1081,.F.) ;
#1440 = ORIENTED_EDGE('',*,*,#1092,.T.) ;
#1441 = ORIENTED_EDGE('',*,*,#1093,.T.) ;
#1442 = ORIENTED_EDGE('',*,*,#1094,.T.) ;
#1443 = ORIENTED_EDGE('',*,*,#1095,.T.) ;
#1444 = ORIENTED_EDGE('',*,*,#1093,.F.) ;
#1445 = ORIENTED_EDGE('',*,*,#1096,.T.) ;
#1446 = ORIENTED_EDGE('',*,*,#1097,.F.) ;
#1447 = ORIENTED_EDGE('',*,*,#1098,.T.) ;
#1448 = ORIENTED_EDGE('',*,*,#1099,.T.) ;
#1449 = ORIENTED_EDGE('',*,*,#1098,.F.) ;
#1450 = ORIENTED_EDGE('',*,*,#1100,.T.) ;
#1451 = ORIENTED_EDGE('',*,*,#1101,.T.) ;
#1452 = ORIENTED_EDGE('',*,*,#1094,.F.) ;
#1453 = ORIENTED_EDGE('',*,*,#1095,.F.) ;
#1454 = ORIENTED_EDGE('',*,*,#1101,.F.) ;
#1455 = ORIENTED_EDGE('',*,*,#1092,.F.) ;
#1456 = ORIENTED_EDGE('',*,*,#1102,.T.) ;
#1457 = ORIENTED_EDGE('',*,*,#1103,.F.) ;
#1458 = ORIENTED_EDGE('',*,*,#1102,.F.) ;
#1459 = ORIENTED_EDGE('',*,*,#1096,.F.) ;
#1460 = ORIENTED_EDGE('',*,*,#1103,.T.) ;
#1461 = ORIENTED_EDGE('',*,*,#1099,.F.) ;
#1462 = ORIENTED_EDGE('',*,*,#1100,.F.) ;
#1463 = ORIENTED_EDGE('',*,*,#1097,.T.) ;
#1464 = ORIENTED_EDGE('',*,*,#1104,.T.) ;
#1465 = ORIENTED_EDGE('',*,*,#1105,.T.) ;
#1466 = ORIENTED_EDGE('',*,*,#1106,.F.) ;
#1467 = ORIENTED_EDGE('',*,*,#1105,.F.) ;
#1468 = ORIENTED_EDGE('',*,*,#1107,.T.) ;
#1469 = ORIENTED_EDGE('',*,*,#1108,.T.) ;
#1470 = ORIENTED_EDGE('',*,*,#1109,.F.) ;
#1471 = ORIENTED_EDGE('',*,*,#1108,.F.) ;
#1472 = ORIENTED_EDGE('',*,*,#1109,.T.) ;
#1473 = ORIENTED_EDGE('',*,*,#1104,.F.) ;
#1474 = ORIENTED_EDGE('',*,*,#1107,.F.) ;
#1475 = ORIENTED_EDGE('',*,*,#1106,.T.) ;
#1476 = ORIENTED_EDGE('',*,*,#1110,.F.) ;
#1477 = ORIENTED_EDGE('',*,*,#1111,.T.) ;
#1478 = ORIENTED_EDGE('',*,*,#1112,.T.) ;
#1479 = ORIENTED_EDGE('',*,*,#1111,.F.) ;
#1480 = ORIENTED_EDGE('',*,*,#1113,.F.) ;
#1481 = ORIENTED_EDGE('',*,*,#1114,.T.) ;
#1482 = ORIENTED_EDGE('',*,*,#1110,.T.) ;
#1483 = ORIENTED_EDGE('',*,*,#1114,.F.) ;
#1484 = ORIENTED_EDGE('',*,*,#1115,.F.) ;
#1485 = ORIENTED_EDGE('',*,*,#1116,.T.) ;
#1486 = ORIENTED_EDGE('',*,*,#1113,.T.) ;
#1487 = ORIENTED_EDGE('',*,*,#1116,.F.) ;
#1488 = ORIENTED_EDGE('',*,*,#1117,.F.) ;
#1489 = ORIENTED_EDGE('',*,*,#1118,.T.) ;
#1490 = ORIENTED_EDGE('',*,*,#1119,.F.) ;
#1491 = ORIENTED_EDGE('',*,*,#1120,.F.) ;
#1492 = ORIENTED_EDGE('',*,*,#1118,.F.) ;
#1493 = ORIENTED_EDGE('',*,*,#1121,.F.) ;
#1494 = ORIENTED_EDGE('',*,*,#1122,.F.) ;
#1495 = ORIENTED_EDGE('',*,*,#1123,.T.) ;
#1496 = ORIENTED_EDGE('',*,*,#1124,.T.) ;
#1497 = ORIENTED_EDGE('',*,*,#1123,.F.) ;
#1498 = ORIENTED_EDGE('',*,*,#1125,.T.) ;
#1499 = ORIENTED_EDGE('',*,*,#1126,.T.) ;
#1500 = ORIENTED_EDGE('',*,*,#1119,.T.) ;
#1501 = ORIENTED_EDGE('',*,*,#1120,.T.) ;
#1502 = ORIENTED_EDGE('',*,*,#1126,.F.) ;
#1503 = ORIENTED_EDGE('',*,*,#1127,.T.) ;
#1504 = ORIENTED_EDGE('',*,*,#1128,.F.) ;
#1505 = ORIENTED_EDGE('',*,*,#1129,.T.) ;
#1506 = ORIENTED_EDGE('',*,*,#1130,.T.) ;
#1507 = ORIENTED_EDGE('',*,*,#1129,.F.) ;
#1508 = ORIENTED_EDGE('',*,*,#1130,.F.) ;
#1509 = ORIENTED_EDGE('',*,*,#1131,.T.) ;
#1510 = ORIENTED_EDGE('',*,*,#1132,.T.) ;
#1511 = ORIENTED_EDGE('',*,*,#1131,.F.) ;
#1512 = ORIENTED_EDGE('',*,*,#1132,.F.) ;
#1513 = ORIENTED_EDGE('',*,*,#1133,.T.) ;
#1514 = ORIENTED_EDGE('',*,*,#1134,.T.) ;
#1515 = ORIENTED_EDGE('',*,*,#1133,.F.) ;
#1516 = ORIENTED_EDGE('',*,*,#1125,.F.) ;
#1517 = ORIENTED_EDGE('',*,*,#1135,.T.) ;
#1518 = ORIENTED_EDGE('',*,*,#1136,.T.) ;
#1519 = ORIENTED_EDGE('',*,*,#1135,.F.) ;
#1520 = ORIENTED_EDGE('',*,*,#1127,.F.) ;
#1521 = ORIENTED_EDGE('',*,*,#1137,.F.) ;
#1522 = ORIENTED_EDGE('',*,*,#1138,.T.) ;
#1523 = ORIENTED_EDGE('',*,*,#1139,.F.) ;
#1524 = ORIENTED_EDGE('',*,*,#1140,.F.) ;
#1525 = ORIENTED_EDGE('',*,*,#1138,.F.) ;
#1526 = ORIENTED_EDGE('',*,*,#1121,.T.) ;
#1527 = ORIENTED_EDGE('',*,*,#1122,.T.) ;
#1528 = ORIENTED_EDGE('',*,*,#1141,.T.) ;
#1529 = ORIENTED_EDGE('',*,*,#1139,.T.) ;
#1530 = ORIENTED_EDGE('',*,*,#1140,.T.) ;
#1531 = ORIENTED_EDGE('',*,*,#1141,.F.) ;
#1532 = ORIENTED_EDGE('',*,*,#1137,.T.) ;
#1533 = ORIENTED_EDGE('',*,*,#1134,.F.) ;
#1534 = ORIENTED_EDGE('',*,*,#1136,.F.) ;
#1535 = ORIENTED_EDGE('',*,*,#1128,.T.) ;
#1536 = ORIENTED_EDGE('',*,*,#1115,.T.) ;
#1537 = ORIENTED_EDGE('',*,*,#1124,.F.) ;
#1538 = ORIENTED_EDGE('',*,*,#1112,.F.) ;
#1539 = ORIENTED_EDGE('',*,*,#1117,.T.) ;
#1540 = ORIENTED_EDGE('',*,*,#1142,.F.) ;
#1541 = ORIENTED_EDGE('',*,*,#1143,.F.) ;
#1542 = ORIENTED_EDGE('',*,*,#1144,.T.) ;
#1543 = ORIENTED_EDGE('',*,*,#1145,.F.) ;
#1544 = ORIENTED_EDGE('',*,*,#1144,.F.) ;
#1545 = ORIENTED_EDGE('',*,*,#1146,.F.) ;
#1546 = ORIENTED_EDGE('',*,*,#1147,.F.) ;
#1547 = ORIENTED_EDGE('',*,*,#1148,.F.) ;
#1548 = ORIENTED_EDGE('',*,*,#1149,.F.) ;
#1549 = ORIENTED_EDGE('',*,*,#1150,.F.) ;
#1550 = ORIENTED_EDGE('',*,*,#1151,.F.) ;
#1551 = ORIENTED_EDGE('',*,*,#1152,.T.) ;
#1552 = ORIENTED_EDGE('',*,*,#1153,.F.) ;
#1553 = ORIENTED_EDGE('',*,*,#1152,.F.) ;
#1554 = ORIENTED_EDGE('',*,*,#1154,.F.) ;
#1555 = ORIENTED_EDGE('',*,*,#1155,.T.) ;
#1556 = ORIENTED_EDGE('',*,*,#1156,.T.) ;
#1557 = ORIENTED_EDGE('',*,*,#1155,.F.) ;
#1558 = ORIENTED_EDGE('',*,*,#1142,.T.) ;
#1559 = ORIENTED_EDGE('',*,*,#1143,.T.) ;
#1560 = ORIENTED_EDGE('',*,*,#1157,.T.) ;
#1561 = ORIENTED_EDGE('',*,*,#1154,.T.) ;
#1562 = ORIENTED_EDGE('',*,*,#1157,.F.) ;
#1563 = ORIENTED_EDGE('',*,*,#1153,.T.) ;
#1564 = ORIENTED_EDGE('',*,*,#1145,.T.) ;
#1565 = ORIENTED_EDGE('',*,*,#1156,.F.) ;
#1566 = ORIENTED_EDGE('',*,*,#1158,.T.) ;
#1567 = ORIENTED_EDGE('',*,*,#1146,.T.) ;
#1568 = ORIENTED_EDGE('',*,*,#1159,.T.) ;
#1569 = ORIENTED_EDGE('',*,*,#1160,.T.) ;
#1570 = ORIENTED_EDGE('',*,*,#1161,.T.) ;
#1571 = ORIENTED_EDGE('',*,*,#1147,.T.) ;
#1572 = ORIENTED_EDGE('',*,*,#1162,.T.) ;
#1573 = ORIENTED_EDGE('',*,*,#1163,.T.) ;
#1574 = ORIENTED_EDGE('',*,*,#1148,.T.) ;
#1575 = ORIENTED_EDGE('',*,*,#1164,.T.) ;
#1576 = ORIENTED_EDGE('',*,*,#1165,.T.) ;
#1577 = ORIENTED_EDGE('',*,*,#1149,.T.) ;
#1578 = ORIENTED_EDGE('',*,*,#1166,.T.) ;
#1579 = ORIENTED_EDGE('',*,*,#1167,.T.) ;
#1580 = ORIENTED_EDGE('',*,*,#1150,.T.) ;
#1581 = ORIENTED_EDGE('',*,*,#1168,.T.) ;
#1582 = ORIENTED_EDGE('',*,*,#1169,.T.) ;
#1583 = ORIENTED_EDGE('',*,*,#1151,.T.) ;
#1584 = ORIENTED_EDGE('',*,*,#1170,.F.) ;
#1585 = ORIENTED_EDGE('',*,*,#1171,.F.) ;
#1586 = ORIENTED_EDGE('',*,*,#1172,.F.) ;
#1587 = ORIENTED_EDGE('',*,*,#1173,.F.) ;
#1588 = ORIENTED_EDGE('',*,*,#1174,.T.) ;
#1589 = ORIENTED_EDGE('',*,*,#1175,.F.) ;
#1590 = ORIENTED_EDGE('',*,*,#1176,.T.) ;
#1591 = ORIENTED_EDGE('',*,*,#1177,.T.) ;
#1592 = ORIENTED_EDGE('',*,*,#1175,.T.) ;
#1593 = ORIENTED_EDGE('',*,*,#1178,.T.) ;
#1594 = ORIENTED_EDGE('',*,*,#1179,.T.) ;
#1595 = ORIENTED_EDGE('',*,*,#1174,.F.) ;
#1596 = ORIENTED_EDGE('',*,*,#1180,.T.) ;
#1597 = ORIENTED_EDGE('',*,*,#1173,.T.) ;
#1598 = ORIENTED_EDGE('',*,*,#1181,.T.) ;
#1599 = ORIENTED_EDGE('',*,*,#1182,.T.) ;
#1600 = ORIENTED_EDGE('',*,*,#1172,.T.) ;
#1601 = ORIENTED_EDGE('',*,*,#1183,.T.) ;
#1602 = ORIENTED_EDGE('',*,*,#1184,.T.) ;
#1603 = ORIENTED_EDGE('',*,*,#1185,.T.) ;
#1604 = ORIENTED_EDGE('',*,*,#1170,.T.) ;
#1605 = ORIENTED_EDGE('',*,*,#1186,.T.) ;
#1606 = ORIENTED_EDGE('',*,*,#1171,.T.) ;
#1607 = ORIENTED_EDGE('',*,*,#1187,.T.) ;
#1608 = ORIENTED_EDGE('',*,*,#1169,.F.) ;
#1609 = ORIENTED_EDGE('',*,*,#1188,.T.) ;
#1610 = ORIENTED_EDGE('',*,*,#1187,.F.) ;
#1611 = ORIENTED_EDGE('',*,*,#1185,.F.) ;
#1612 = ORIENTED_EDGE('',*,*,#1189,.F.) ;
#1613 = ORIENTED_EDGE('',*,*,#1159,.F.) ;
#1614 = ORIENTED_EDGE('',*,*,#1167,.F.) ;
#1615 = ORIENTED_EDGE('',*,*,#1190,.T.) ;
#1616 = ORIENTED_EDGE('',*,*,#1183,.F.) ;
#1617 = ORIENTED_EDGE('',*,*,#1186,.F.) ;
#1618 = ORIENTED_EDGE('',*,*,#1188,.F.) ;
#1619 = ORIENTED_EDGE('',*,*,#1168,.F.) ;
#1620 = ORIENTED_EDGE('',*,*,#1165,.F.) ;
#1621 = ORIENTED_EDGE('',*,*,#1191,.T.) ;
#1622 = ORIENTED_EDGE('',*,*,#1181,.F.) ;
#1623 = ORIENTED_EDGE('',*,*,#1182,.F.) ;
#1624 = ORIENTED_EDGE('',*,*,#1190,.F.) ;
#1625 = ORIENTED_EDGE('',*,*,#1166,.F.) ;
#1626 = ORIENTED_EDGE('',*,*,#1163,.F.) ;
#1627 = ORIENTED_EDGE('',*,*,#1192,.T.) ;
#1628 = ORIENTED_EDGE('',*,*,#1178,.F.) ;
#1629 = ORIENTED_EDGE('',*,*,#1180,.F.) ;
#1630 = ORIENTED_EDGE('',*,*,#1191,.F.) ;
#1631 = ORIENTED_EDGE('',*,*,#1164,.F.) ;
#1632 = ORIENTED_EDGE('',*,*,#1161,.F.) ;
#1633 = ORIENTED_EDGE('',*,*,#1193,.T.) ;
#1634 = ORIENTED_EDGE('',*,*,#1176,.F.) ;
#1635 = ORIENTED_EDGE('',*,*,#1179,.F.) ;
#1636 = ORIENTED_EDGE('',*,*,#1192,.F.) ;
#1637 = ORIENTED_EDGE('',*,*,#1162,.F.) ;
#1638 = ORIENTED_EDGE('',*,*,#1158,.F.) ;
#1639 = ORIENTED_EDGE('',*,*,#1189,.T.) ;
#1640 = ORIENTED_EDGE('',*,*,#1184,.F.) ;
#1641 = ORIENTED_EDGE('',*,*,#1177,.F.) ;
#1642 = ORIENTED_EDGE('',*,*,#1193,.F.) ;
#1643 = ORIENTED_EDGE('',*,*,#1160,.F.) ;
#1644 = PLANE('',#1972) ;
#1645 = PLANE('',#1973) ;
#1646 = PLANE('',#1974) ;
#1647 = PLANE('',#1975) ;
#1648 = PLANE('',#1976) ;
#1649 = PLANE('',#1977) ;
#1650 = PLANE('',#1982) ;
#1651 = PLANE('',#1983) ;
#1652 = PLANE('',#1984) ;
#1653 = PLANE('',#1985) ;
#1654 = PLANE('',#1986) ;
#1655 = PLANE('',#1987) ;
#1656 = PLANE('',#1995) ;
#1657 = PLANE('',#1996) ;
#1658 = PLANE('',#1997) ;
#1659 = PLANE('',#1998) ;
#1660 = PLANE('',#1999) ;
#1661 = PLANE('',#2000) ;
#1662 = PLANE('',#2001) ;
#1663 = PLANE('',#2002) ;
#1664 = PLANE('',#2003) ;
#1665 = PLANE('',#2004) ;
#1666 = PLANE('',#2005) ;
#1667 = PLANE('',#2006) ;
#1668 = PLANE('',#2021) ;
#1669 = PLANE('',#2022) ;
#1670 = PLANE('',#2027) ;
#1671 = PLANE('',#2028) ;
#1672 = PLANE('',#2036) ;
#1673 = PLANE('',#2037) ;
#1674 = PLANE('',#2038) ;
#1675 = PLANE('',#2039) ;
#1676 = PLANE('',#2040) ;
#1677 = PLANE('',#2041) ;
#1678 = PLANE('',#2042) ;
#1679 = PLANE('',#2057) ;
#1680 = PLANE('',#2058) ;
#1681 = PLANE('',#2059) ;
#1682 = PLANE('',#2060) ;
#1683 = PLANE('',#2075) ;
#1684 = PLANE('',#2076) ;
#1685 = PLANE('',#2077) ;
#1686 = PLANE('',#2078) ;
#1687 = PLANE('',#2100) ;
#1688 = PLANE('',#2101) ;
#1689 = PLANE('',#2109) ;
#1690 = PLANE('',#2110) ;
#1691 = PLANE('',#2157) ;
#1692 = PLANE('',#2158) ;
#1693 = PLANE('',#2159) ;
#1694 = PLANE('',#2160) ;
#1695 = PLANE('',#2179) ;
#1696 = PLANE('',#2180) ;
#1697 = PLANE('',#2181) ;
#1698 = PLANE('',#2182) ;
#1699 = PLANE('',#2183) ;
#1700 = PLANE('',#2184) ;
#1701 = PLANE('',#2185) ;
#1702 = PLANE('',#2186) ;
#1703 = PLANE('',#2187) ;
#1704 = PLANE('',#2200) ;
#1705 = PLANE('',#2201) ;
#1706 = PLANE('',#2202) ;
#1707 = PLANE('',#2203) ;
#1708 = PLANE('',#2204) ;
#1709 = PLANE('',#2205) ;
#1710 = ADVANCED_FACE('',(#334),#1644,.T.) ;
#1711 = ADVANCED_FACE('',(#335),#1645,.T.) ;
#1712 = ADVANCED_FACE('',(#336),#1646,.T.) ;
#1713 = ADVANCED_FACE('',(#337),#1647,.T.) ;
#1714 = ADVANCED_FACE('',(#338),#1648,.F.) ;
#1715 = ADVANCED_FACE('',(#339),#1649,.T.) ;
#1716 = ADVANCED_FACE('',(#340),#256,.F.) ;
#1717 = ADVANCED_FACE('',(#341),#1650,.T.) ;
#1718 = ADVANCED_FACE('',(#342),#1651,.T.) ;
#1719 = ADVANCED_FACE('',(#343),#1652,.T.) ;
#1720 = ADVANCED_FACE('',(#344),#1653,.T.) ;
#1721 = ADVANCED_FACE('',(#345,#141),#1654,.F.) ;
#1722 = ADVANCED_FACE('',(#346,#142),#1655,.T.) ;
#1723 = ADVANCED_FACE('',(#347),#257,.F.) ;
#1724 = ADVANCED_FACE('',(#348),#258,.F.) ;
#1725 = ADVANCED_FACE('',(#349),#1656,.T.) ;
#1726 = ADVANCED_FACE('',(#350),#1657,.T.) ;
#1727 = ADVANCED_FACE('',(#351),#1658,.T.) ;
#1728 = ADVANCED_FACE('',(#352),#1659,.T.) ;
#1729 = ADVANCED_FACE('',(#353),#1660,.T.) ;
#1730 = ADVANCED_FACE('',(#354),#1661,.T.) ;
#1731 = ADVANCED_FACE('',(#355),#1662,.T.) ;
#1732 = ADVANCED_FACE('',(#356,#143,#144),#1663,.F.) ;
#1733 = ADVANCED_FACE('',(#357,#145,#146),#1664,.T.) ;
#1734 = ADVANCED_FACE('',(#358),#1665,.F.) ;
#1735 = ADVANCED_FACE('',(#359),#1666,.F.) ;
#1736 = ADVANCED_FACE('',(#360),#1667,.F.) ;
#1737 = ADVANCED_FACE('',(#361),#259,.F.) ;
#1738 = ADVANCED_FACE('',(#362),#31,.T.) ;
#1739 = ADVANCED_FACE('',(#363,#147),#260,.T.) ;
#1740 = ADVANCED_FACE('',(#364),#261,.T.) ;
#1741 = ADVANCED_FACE('',(#365),#1668,.T.) ;
#1742 = ADVANCED_FACE('',(#366),#1669,.T.) ;
#1743 = ADVANCED_FACE('',(#367),#262,.T.) ;
#1744 = ADVANCED_FACE('',(#368),#1670,.T.) ;
#1745 = ADVANCED_FACE('',(#369),#1671,.F.) ;
#1746 = ADVANCED_FACE('',(#370),#263,.F.) ;
#1747 = ADVANCED_FACE('',(#371),#264,.F.) ;
#1748 = ADVANCED_FACE('',(#372,#148),#1672,.F.) ;
#1749 = ADVANCED_FACE('',(#373),#1673,.F.) ;
#1750 = ADVANCED_FACE('',(#374,#149),#1674,.F.) ;
#1751 = ADVANCED_FACE('',(#375,#150),#1675,.F.) ;
#1752 = ADVANCED_FACE('',(#376),#1676,.T.) ;
#1753 = ADVANCED_FACE('',(#377),#1677,.F.) ;
#1754 = ADVANCED_FACE('',(#378),#1678,.T.) ;
#1755 = ADVANCED_FACE('',(#379),#265,.F.) ;
#1756 = ADVANCED_FACE('',(#380),#32,.F.) ;
#1757 = ADVANCED_FACE('',(#381),#266,.T.) ;
#1758 = ADVANCED_FACE('',(#382),#267,.T.) ;
#1759 = ADVANCED_FACE('',(#383),#268,.T.) ;
#1760 = ADVANCED_FACE('',(#384),#1679,.T.) ;
#1761 = ADVANCED_FACE('',(#385,#151),#1680,.T.) ;
#1762 = ADVANCED_FACE('',(#386,#152),#1681,.T.) ;
#1763 = ADVANCED_FACE('',(#387,#153),#1682,.T.) ;
#1764 = ADVANCED_FACE('',(#388),#269,.F.) ;
#1765 = ADVANCED_FACE('',(#389),#33,.F.) ;
#1766 = ADVANCED_FACE('',(#390),#270,.T.) ;
#1767 = ADVANCED_FACE('',(#391),#271,.T.) ;
#1768 = ADVANCED_FACE('',(#392),#272,.T.) ;
#1769 = ADVANCED_FACE('',(#393),#1683,.T.) ;
#1770 = ADVANCED_FACE('',(#394,#154),#1684,.T.) ;
#1771 = ADVANCED_FACE('',(#395,#155),#1685,.T.) ;
#1772 = ADVANCED_FACE('',(#396,#156),#1686,.T.) ;
#1773 = ADVANCED_FACE('',(#397),#23,.F.) ;
#1774 = ADVANCED_FACE('',(#398),#273,.F.) ;
#1775 = ADVANCED_FACE('',(#399),#274,.T.) ;
#1776 = ADVANCED_FACE('',(#400),#275,.T.) ;
#1777 = ADVANCED_FACE('',(#401,#157),#1687,.T.) ;
#1778 = ADVANCED_FACE('',(#402,#158),#1688,.F.) ;
#1779 = ADVANCED_FACE('',(#403),#276,.F.) ;
#1780 = ADVANCED_FACE('',(#404),#277,.T.) ;
#1781 = ADVANCED_FACE('',(#405,#159),#1689,.T.) ;
#1782 = ADVANCED_FACE('',(#406,#160),#1690,.F.) ;
#1783 = ADVANCED_FACE('',(#407),#24,.T.) ;
#1784 = ADVANCED_FACE('',(#408),#278,.T.) ;
#1785 = ADVANCED_FACE('',(#409),#25,.T.) ;
#1786 = ADVANCED_FACE('',(#410),#279,.F.) ;
#1787 = ADVANCED_FACE('',(#411),#280,.F.) ;
#1788 = ADVANCED_FACE('',(#412),#26,.T.) ;
#1789 = ADVANCED_FACE('',(#413),#27,.T.) ;
#1790 = ADVANCED_FACE('',(#414),#281,.F.) ;
#1791 = ADVANCED_FACE('',(#415),#28,.T.) ;
#1792 = ADVANCED_FACE('',(#416),#282,.T.) ;
#1793 = ADVANCED_FACE('',(#417),#283,.T.) ;
#1794 = ADVANCED_FACE('',(#418),#29,.T.) ;
#1795 = ADVANCED_FACE('',(#419,#161),#1691,.T.) ;
#1796 = ADVANCED_FACE('',(#420,#162),#1692,.T.) ;
#1797 = ADVANCED_FACE('',(#421,#163),#1693,.T.) ;
#1798 = ADVANCED_FACE('',(#422,#164),#1694,.T.) ;
#1799 = ADVANCED_FACE('',(#423),#30,.F.) ;
#1800 = ADVANCED_FACE('',(#424),#284,.T.) ;
#1801 = ADVANCED_FACE('',(#425),#34,.T.) ;
#1802 = ADVANCED_FACE('',(#426),#285,.T.) ;
#1803 = ADVANCED_FACE('',(#427,#165),#1695,.T.) ;
#1804 = ADVANCED_FACE('',(#428),#1696,.F.) ;
#1805 = ADVANCED_FACE('',(#429),#1697,.T.) ;
#1806 = ADVANCED_FACE('',(#430),#1698,.T.) ;
#1807 = ADVANCED_FACE('',(#431),#1699,.T.) ;
#1808 = ADVANCED_FACE('',(#432),#1700,.T.) ;
#1809 = ADVANCED_FACE('',(#433),#1701,.T.) ;
#1810 = ADVANCED_FACE('',(#434),#1702,.T.) ;
#1811 = ADVANCED_FACE('',(#435),#1703,.F.) ;
#1812 = ADVANCED_FACE('',(#436),#35,.T.) ;
#1813 = ADVANCED_FACE('',(#437),#36,.T.) ;
#1814 = ADVANCED_FACE('',(#438),#37,.T.) ;
#1815 = ADVANCED_FACE('',(#439),#38,.T.) ;
#1816 = ADVANCED_FACE('',(#440),#39,.T.) ;
#1817 = ADVANCED_FACE('',(#441),#40,.T.) ;
#1818 = ADVANCED_FACE('',(#442),#1704,.F.) ;
#1819 = ADVANCED_FACE('',(#443),#1705,.F.) ;
#1820 = ADVANCED_FACE('',(#444),#1706,.F.) ;
#1821 = ADVANCED_FACE('',(#445),#1707,.F.) ;
#1822 = ADVANCED_FACE('',(#446),#1708,.F.) ;
#1823 = ADVANCED_FACE('',(#447),#1709,.F.) ;
#1824 = CLOSED_SHELL('',(#1710,#1711,#1712,#1713,#1714,#1715)) ;
#1825 = CLOSED_SHELL('',(#1716,#1717,#1718,#1719,#1720,#1721,#1722)) ;
#1826 = CLOSED_SHELL('',(#1723,#1724,#1725,#1726,#1727,#1728,#1729,#1730,
#1731,#1732,#1733,#1734,#1735,#1736)) ;
#1827 = CLOSED_SHELL('',(#1737,#1738,#1739,#1740,#1741,#1742)) ;
#1828 = CLOSED_SHELL('',(#1743,#1744,#1745)) ;
#1829 = CLOSED_SHELL('',(#1746,#1747,#1748,#1749,#1750,#1751,#1752,#1753,
#1754)) ;
#1830 = CLOSED_SHELL('',(#1755,#1756,#1757,#1758,#1759,#1760,#1761,#1762,
#1763)) ;
#1831 = CLOSED_SHELL('',(#1764,#1765,#1766,#1767,#1768,#1769,#1770,#1771,
#1772)) ;
#1832 = CLOSED_SHELL('',(#1773,#1774,#1775,#1776,#1777,#1778)) ;
#1833 = CLOSED_SHELL('',(#1779,#1780,#1781,#1782)) ;
#1834 = CLOSED_SHELL('',(#1783,#1784,#1785,#1786,#1787,#1788,#1789,#1790,
#1791,#1792,#1793,#1794,#1795,#1796,#1797,#1798)) ;
#1835 = CLOSED_SHELL('',(#1799,#1800,#1801,#1802,#1803,#1804,#1805,#1806,
#1807,#1808,#1809,#1810,#1811,#1812,#1813,#1814,#1815,#1816,#1817,#1818,
#1819,#1820,#1821,#1822,#1823)) ;
#1836 = DERIVED_UNIT_ELEMENT(#1860,1.) ;
#1837 = DERIVED_UNIT_ELEMENT(#3477,-3.) ;
#1838 = DERIVED_UNIT_ELEMENT(#1860,1.) ;
#1839 = DERIVED_UNIT_ELEMENT(#3477,-3.) ;
#1840 = DERIVED_UNIT_ELEMENT(#1860,1.) ;
#1841 = DERIVED_UNIT_ELEMENT(#3477,-3.) ;
#1842 = DERIVED_UNIT_ELEMENT(#1860,1.) ;
#1843 = DERIVED_UNIT_ELEMENT(#3477,-3.) ;
#1844 = DERIVED_UNIT_ELEMENT(#1860,1.) ;
#1845 = DERIVED_UNIT_ELEMENT(#3477,-3.) ;
#1846 = DERIVED_UNIT_ELEMENT(#1860,1.) ;
#1847 = DERIVED_UNIT_ELEMENT(#3477,-3.) ;
#1848 = DERIVED_UNIT_ELEMENT(#1860,1.) ;
#1849 = DERIVED_UNIT_ELEMENT(#3477,-3.) ;
#1850 = DERIVED_UNIT_ELEMENT(#1860,1.) ;
#1851 = DERIVED_UNIT_ELEMENT(#3477,-3.) ;
#1852 = DERIVED_UNIT_ELEMENT(#1860,1.) ;
#1853 = DERIVED_UNIT_ELEMENT(#3477,-3.) ;
#1854 = DERIVED_UNIT_ELEMENT(#1860,1.) ;
#1855 = DERIVED_UNIT_ELEMENT(#3477,-3.) ;
#1856 = DERIVED_UNIT_ELEMENT(#1860,1.) ;
#1857 = DERIVED_UNIT_ELEMENT(#3477,-3.) ;
#1858 = DERIVED_UNIT_ELEMENT(#1860,1.) ;
#1859 = DERIVED_UNIT_ELEMENT(#3477,-3.) ;
#1860 = (
MASS_UNIT()
NAMED_UNIT(*)
SI_UNIT(.KILO.,.GRAM.)
) ;
#1861 = DERIVED_UNIT((#1836,#1837)) ;
#1862 = DERIVED_UNIT((#1838,#1839)) ;
#1863 = DERIVED_UNIT((#1840,#1841)) ;
#1864 = DERIVED_UNIT((#1842,#1843)) ;
#1865 = DERIVED_UNIT((#1844,#1845)) ;
#1866 = DERIVED_UNIT((#1846,#1847)) ;
#1867 = DERIVED_UNIT((#1848,#1849)) ;
#1868 = DERIVED_UNIT((#1850,#1851)) ;
#1869 = DERIVED_UNIT((#1852,#1853)) ;
#1870 = DERIVED_UNIT((#1854,#1855)) ;
#1871 = DERIVED_UNIT((#1856,#1857)) ;
#1872 = DERIVED_UNIT((#1858,#1859)) ;
#1873 = MEASURE_REPRESENTATION_ITEM('density measure',
POSITIVE_RATIO_MEASURE(7850.),#1861) ;
#1874 = MEASURE_REPRESENTATION_ITEM('density measure',
POSITIVE_RATIO_MEASURE(7850.),#1862) ;
#1875 = MEASURE_REPRESENTATION_ITEM('density measure',
POSITIVE_RATIO_MEASURE(7850.),#1863) ;
#1876 = MEASURE_REPRESENTATION_ITEM('density measure',
POSITIVE_RATIO_MEASURE(7850.),#1864) ;
#1877 = MEASURE_REPRESENTATION_ITEM('density measure',
POSITIVE_RATIO_MEASURE(7850.),#1865) ;
#1878 = MEASURE_REPRESENTATION_ITEM('density measure',
POSITIVE_RATIO_MEASURE(7850.),#1866) ;
#1879 = MEASURE_REPRESENTATION_ITEM('density measure',
POSITIVE_RATIO_MEASURE(7850.),#1867) ;
#1880 = MEASURE_REPRESENTATION_ITEM('density measure',
POSITIVE_RATIO_MEASURE(7850.),#1868) ;
#1881 = MEASURE_REPRESENTATION_ITEM('density measure',
POSITIVE_RATIO_MEASURE(7850.),#1869) ;
#1882 = MEASURE_REPRESENTATION_ITEM('density measure',
POSITIVE_RATIO_MEASURE(7850.),#1870) ;
#1883 = MEASURE_REPRESENTATION_ITEM('density measure',
POSITIVE_RATIO_MEASURE(7850.),#1871) ;
#1884 = MEASURE_REPRESENTATION_ITEM('density measure',
POSITIVE_RATIO_MEASURE(7850.),#1872) ;
#1885 = PROPERTY_DEFINITION_REPRESENTATION(#1945,#1909) ;
#1886 = PROPERTY_DEFINITION_REPRESENTATION(#1946,#1910) ;
#1887 = PROPERTY_DEFINITION_REPRESENTATION(#1947,#1911) ;
#1888 = PROPERTY_DEFINITION_REPRESENTATION(#1948,#1912) ;
#1889 = PROPERTY_DEFINITION_REPRESENTATION(#1949,#1913) ;
#1890 = PROPERTY_DEFINITION_REPRESENTATION(#1950,#1914) ;
#1891 = PROPERTY_DEFINITION_REPRESENTATION(#1951,#1915) ;
#1892 = PROPERTY_DEFINITION_REPRESENTATION(#1952,#1916) ;
#1893 = PROPERTY_DEFINITION_REPRESENTATION(#1953,#1917) ;
#1894 = PROPERTY_DEFINITION_REPRESENTATION(#1954,#1918) ;
#1895 = PROPERTY_DEFINITION_REPRESENTATION(#1955,#1919) ;
#1896 = PROPERTY_DEFINITION_REPRESENTATION(#1956,#1920) ;
#1897 = PROPERTY_DEFINITION_REPRESENTATION(#1957,#1921) ;
#1898 = PROPERTY_DEFINITION_REPRESENTATION(#1958,#1922) ;
#1899 = PROPERTY_DEFINITION_REPRESENTATION(#1959,#1923) ;
#1900 = PROPERTY_DEFINITION_REPRESENTATION(#1960,#1924) ;
#1901 = PROPERTY_DEFINITION_REPRESENTATION(#1961,#1925) ;
#1902 = PROPERTY_DEFINITION_REPRESENTATION(#1962,#1926) ;
#1903 = PROPERTY_DEFINITION_REPRESENTATION(#1963,#1927) ;
#1904 = PROPERTY_DEFINITION_REPRESENTATION(#1964,#1928) ;
#1905 = PROPERTY_DEFINITION_REPRESENTATION(#1965,#1929) ;
#1906 = PROPERTY_DEFINITION_REPRESENTATION(#1966,#1930) ;
#1907 = PROPERTY_DEFINITION_REPRESENTATION(#1967,#1931) ;
#1908 = PROPERTY_DEFINITION_REPRESENTATION(#1968,#1932) ;
#1909 = REPRESENTATION('material name',(#1933),#3460) ;
#1910 = REPRESENTATION('density',(#1873),#3460) ;
#1911 = REPRESENTATION('material name',(#1934),#3461) ;
#1912 = REPRESENTATION('density',(#1874),#3461) ;
#1913 = REPRESENTATION('material name',(#1935),#3462) ;
#1914 = REPRESENTATION('density',(#1875),#3462) ;
#1915 = REPRESENTATION('material name',(#1936),#3464) ;
#1916 = REPRESENTATION('density',(#1876),#3464) ;
#1917 = REPRESENTATION('material name',(#1937),#3465) ;
#1918 = REPRESENTATION('density',(#1877),#3465) ;
#1919 = REPRESENTATION('material name',(#1938),#3466) ;
#1920 = REPRESENTATION('density',(#1878),#3466) ;
#1921 = REPRESENTATION('material name',(#1939),#3467) ;
#1922 = REPRESENTATION('density',(#1879),#3467) ;
#1923 = REPRESENTATION('material name',(#1940),#3468) ;
#1924 = REPRESENTATION('density',(#1880),#3468) ;
#1925 = REPRESENTATION('material name',(#1941),#3470) ;
#1926 = REPRESENTATION('density',(#1881),#3470) ;
#1927 = REPRESENTATION('material name',(#1942),#3471) ;
#1928 = REPRESENTATION('density',(#1882),#3471) ;
#1929 = REPRESENTATION('material name',(#1943),#3473) ;
#1930 = REPRESENTATION('density',(#1883),#3473) ;
#1931 = REPRESENTATION('material name',(#1944),#3474) ;
#1932 = REPRESENTATION('density',(#1884),#3474) ;
#1933 = DESCRIPTIVE_REPRESENTATION_ITEM('Steel','Steel') ;
#1934 = DESCRIPTIVE_REPRESENTATION_ITEM('Steel','Steel') ;
#1935 = DESCRIPTIVE_REPRESENTATION_ITEM('Steel','Steel') ;
#1936 = DESCRIPTIVE_REPRESENTATION_ITEM('Steel','Steel') ;
#1937 = DESCRIPTIVE_REPRESENTATION_ITEM('Steel','Steel') ;
#1938 = DESCRIPTIVE_REPRESENTATION_ITEM('Steel','Steel') ;
#1939 = DESCRIPTIVE_REPRESENTATION_ITEM('Steel','Steel') ;
#1940 = DESCRIPTIVE_REPRESENTATION_ITEM('Steel','Steel') ;
#1941 = DESCRIPTIVE_REPRESENTATION_ITEM('Steel','Steel') ;
#1942 = DESCRIPTIVE_REPRESENTATION_ITEM('Steel','Steel') ;
#1943 = DESCRIPTIVE_REPRESENTATION_ITEM('Steel','Steel') ;
#1944 = DESCRIPTIVE_REPRESENTATION_ITEM('Steel','Steel') ;
#1945 = PROPERTY_DEFINITION('material property','material name',#3558) ;
#1946 = PROPERTY_DEFINITION('material property','density of part',#3558) ;
#1947 = PROPERTY_DEFINITION('material property','material name',#3559) ;
#1948 = PROPERTY_DEFINITION('material property','density of part',#3559) ;
#1949 = PROPERTY_DEFINITION('material property','material name',#3560) ;
#1950 = PROPERTY_DEFINITION('material property','density of part',#3560) ;
#1951 = PROPERTY_DEFINITION('material property','material name',#3562) ;
#1952 = PROPERTY_DEFINITION('material property','density of part',#3562) ;
#1953 = PROPERTY_DEFINITION('material property','material name',#3563) ;
#1954 = PROPERTY_DEFINITION('material property','density of part',#3563) ;
#1955 = PROPERTY_DEFINITION('material property','material name',#3564) ;
#1956 = PROPERTY_DEFINITION('material property','density of part',#3564) ;
#1957 = PROPERTY_DEFINITION('material property','material name',#3565) ;
#1958 = PROPERTY_DEFINITION('material property','density of part',#3565) ;
#1959 = PROPERTY_DEFINITION('material property','material name',#3566) ;
#1960 = PROPERTY_DEFINITION('material property','density of part',#3566) ;
#1961 = PROPERTY_DEFINITION('material property','material name',#3568) ;
#1962 = PROPERTY_DEFINITION('material property','density of part',#3568) ;
#1963 = PROPERTY_DEFINITION('material property','material name',#3569) ;
#1964 = PROPERTY_DEFINITION('material property','density of part',#3569) ;
#1965 = PROPERTY_DEFINITION('material property','material name',#3571) ;
#1966 = PROPERTY_DEFINITION('material property','density of part',#3571) ;
#1967 = PROPERTY_DEFINITION('material property','material name',#3572) ;
#1968 = PROPERTY_DEFINITION('material property','density of part',#3572) ;
#1969 = AXIS2_PLACEMENT_3D('',#2823,#2214,#2215) ;
#1970 = AXIS2_PLACEMENT_3D('',#2824,#2216,#2217) ;
#1971 = AXIS2_PLACEMENT_3D('',#2825,#2218,#2219) ;
#1972 = AXIS2_PLACEMENT_3D('',#2826,#2220,#2221) ;
#1973 = AXIS2_PLACEMENT_3D('',#2835,#2226,#2227) ;
#1974 = AXIS2_PLACEMENT_3D('',#2841,#2231,#2232) ;
#1975 = AXIS2_PLACEMENT_3D('',#2847,#2236,#2237) ;
#1976 = AXIS2_PLACEMENT_3D('',#2850,#2240,#2241) ;
#1977 = AXIS2_PLACEMENT_3D('',#2851,#2242,#2243) ;
#1978 = AXIS2_PLACEMENT_3D('',#2852,#2244,#2245) ;
#1979 = AXIS2_PLACEMENT_3D('',#2853,#2246,#2247) ;
#1980 = AXIS2_PLACEMENT_3D('',#2855,#2248,#2249) ;
#1981 = AXIS2_PLACEMENT_3D('',#2858,#2251,#2252) ;
#1982 = AXIS2_PLACEMENT_3D('',#2859,#2253,#2254) ;
#1983 = AXIS2_PLACEMENT_3D('',#2868,#2259,#2260) ;
#1984 = AXIS2_PLACEMENT_3D('',#2874,#2264,#2265) ;
#1985 = AXIS2_PLACEMENT_3D('',#2880,#2269,#2270) ;
#1986 = AXIS2_PLACEMENT_3D('',#2883,#2273,#2274) ;
#1987 = AXIS2_PLACEMENT_3D('',#2884,#2275,#2276) ;
#1988 = AXIS2_PLACEMENT_3D('',#2885,#2277,#2278) ;
#1989 = AXIS2_PLACEMENT_3D('',#2886,#2279,#2280) ;
#1990 = AXIS2_PLACEMENT_3D('',#2888,#2281,#2282) ;
#1991 = AXIS2_PLACEMENT_3D('',#2891,#2284,#2285) ;
#1992 = AXIS2_PLACEMENT_3D('',#2892,#2286,#2287) ;
#1993 = AXIS2_PLACEMENT_3D('',#2894,#2288,#2289) ;
#1994 = AXIS2_PLACEMENT_3D('',#2897,#2291,#2292) ;
#1995 = AXIS2_PLACEMENT_3D('',#2898,#2293,#2294) ;
#1996 = AXIS2_PLACEMENT_3D('',#2907,#2299,#2300) ;
#1997 = AXIS2_PLACEMENT_3D('',#2916,#2305,#2306) ;
#1998 = AXIS2_PLACEMENT_3D('',#2922,#2310,#2311) ;
#1999 = AXIS2_PLACEMENT_3D('',#2928,#2315,#2316) ;
#2000 = AXIS2_PLACEMENT_3D('',#2934,#2320,#2321) ;
#2001 = AXIS2_PLACEMENT_3D('',#2940,#2325,#2326) ;
#2002 = AXIS2_PLACEMENT_3D('',#2943,#2329,#2330) ;
#2003 = AXIS2_PLACEMENT_3D('',#2949,#2334,#2335) ;
#2004 = AXIS2_PLACEMENT_3D('',#2955,#2339,#2340) ;
#2005 = AXIS2_PLACEMENT_3D('',#2958,#2343,#2344) ;
#2006 = AXIS2_PLACEMENT_3D('',#2959,#2345,#2346) ;
#2007 = AXIS2_PLACEMENT_3D('',#2960,#2347,#2348) ;
#2008 = AXIS2_PLACEMENT_3D('',#2961,#2349,#2350) ;
#2009 = AXIS2_PLACEMENT_3D('',#2962,#2351,#2352) ;
#2010 = AXIS2_PLACEMENT_3D('',#2963,#2353,#2354) ;
#2011 = AXIS2_PLACEMENT_3D('',#2964,#2355,#2356) ;
#2012 = AXIS2_PLACEMENT_3D('',#2965,#2357,#2358) ;
#2013 = AXIS2_PLACEMENT_3D('',#2966,#2359,#2360) ;
#2014 = AXIS2_PLACEMENT_3D('',#3045,#2362,#2363) ;
#2015 = AXIS2_PLACEMENT_3D('',#3047,#2364,#2365) ;
#2016 = AXIS2_PLACEMENT_3D('',#3050,#2367,#2368) ;
#2017 = AXIS2_PLACEMENT_3D('',#3051,#2369,#2370) ;
#2018 = AXIS2_PLACEMENT_3D('',#3053,#2371,#2372) ;
#2019 = AXIS2_PLACEMENT_3D('',#3056,#2375,#2376) ;
#2020 = AXIS2_PLACEMENT_3D('',#3059,#2378,#2379) ;
#2021 = AXIS2_PLACEMENT_3D('',#3060,#2380,#2381) ;
#2022 = AXIS2_PLACEMENT_3D('',#3061,#2382,#2383) ;
#2023 = AXIS2_PLACEMENT_3D('',#3062,#2384,#2385) ;
#2024 = AXIS2_PLACEMENT_3D('',#3063,#2386,#2387) ;
#2025 = AXIS2_PLACEMENT_3D('',#3065,#2388,#2389) ;
#2026 = AXIS2_PLACEMENT_3D('',#3068,#2391,#2392) ;
#2027 = AXIS2_PLACEMENT_3D('',#3069,#2393,#2394) ;
#2028 = AXIS2_PLACEMENT_3D('',#3070,#2395,#2396) ;
#2029 = AXIS2_PLACEMENT_3D('',#3071,#2397,#2398) ;
#2030 = AXIS2_PLACEMENT_3D('',#3072,#2399,#2400) ;
#2031 = AXIS2_PLACEMENT_3D('',#3074,#2401,#2402) ;
#2032 = AXIS2_PLACEMENT_3D('',#3077,#2404,#2405) ;
#2033 = AXIS2_PLACEMENT_3D('',#3078,#2406,#2407) ;
#2034 = AXIS2_PLACEMENT_3D('',#3080,#2408,#2409) ;
#2035 = AXIS2_PLACEMENT_3D('',#3083,#2411,#2412) ;
#2036 = AXIS2_PLACEMENT_3D('',#3084,#2413,#2414) ;
#2037 = AXIS2_PLACEMENT_3D('',#3093,#2419,#2420) ;
#2038 = AXIS2_PLACEMENT_3D('',#3099,#2424,#2425) ;
#2039 = AXIS2_PLACEMENT_3D('',#3105,#2429,#2430) ;
#2040 = AXIS2_PLACEMENT_3D('',#3108,#2433,#2434) ;
#2041 = AXIS2_PLACEMENT_3D('',#3109,#2435,#2436) ;
#2042 = AXIS2_PLACEMENT_3D('',#3110,#2437,#2438) ;
#2043 = AXIS2_PLACEMENT_3D('',#3111,#2439,#2440) ;
#2044 = AXIS2_PLACEMENT_3D('',#3112,#2441,#2442) ;
#2045 = AXIS2_PLACEMENT_3D('',#3114,#2443,#2444) ;
#2046 = AXIS2_PLACEMENT_3D('',#3117,#2446,#2447) ;
#2047 = AXIS2_PLACEMENT_3D('',#3118,#2448,#2449) ;
#2048 = AXIS2_PLACEMENT_3D('',#3121,#2451,#2452) ;
#2049 = AXIS2_PLACEMENT_3D('',#3123,#2453,#2454) ;
#2050 = AXIS2_PLACEMENT_3D('',#3126,#2456,#2457) ;
#2051 = AXIS2_PLACEMENT_3D('',#3127,#2458,#2459) ;
#2052 = AXIS2_PLACEMENT_3D('',#3129,#2460,#2461) ;
#2053 = AXIS2_PLACEMENT_3D('',#3132,#2463,#2464) ;
#2054 = AXIS2_PLACEMENT_3D('',#3133,#2465,#2466) ;
#2055 = AXIS2_PLACEMENT_3D('',#3135,#2467,#2468) ;
#2056 = AXIS2_PLACEMENT_3D('',#3138,#2470,#2471) ;
#2057 = AXIS2_PLACEMENT_3D('',#3139,#2472,#2473) ;
#2058 = AXIS2_PLACEMENT_3D('',#3140,#2474,#2475) ;
#2059 = AXIS2_PLACEMENT_3D('',#3141,#2476,#2477) ;
#2060 = AXIS2_PLACEMENT_3D('',#3142,#2478,#2479) ;
#2061 = AXIS2_PLACEMENT_3D('',#3143,#2480,#2481) ;
#2062 = AXIS2_PLACEMENT_3D('',#3144,#2482,#2483) ;
#2063 = AXIS2_PLACEMENT_3D('',#3146,#2484,#2485) ;
#2064 = AXIS2_PLACEMENT_3D('',#3149,#2487,#2488) ;
#2065 = AXIS2_PLACEMENT_3D('',#3150,#2489,#2490) ;
#2066 = AXIS2_PLACEMENT_3D('',#3153,#2492,#2493) ;
#2067 = AXIS2_PLACEMENT_3D('',#3155,#2494,#2495) ;
#2068 = AXIS2_PLACEMENT_3D('',#3158,#2497,#2498) ;
#2069 = AXIS2_PLACEMENT_3D('',#3159,#2499,#2500) ;
#2070 = AXIS2_PLACEMENT_3D('',#3161,#2501,#2502) ;
#2071 = AXIS2_PLACEMENT_3D('',#3164,#2504,#2505) ;
#2072 = AXIS2_PLACEMENT_3D('',#3165,#2506,#2507) ;
#2073 = AXIS2_PLACEMENT_3D('',#3167,#2508,#2509) ;
#2074 = AXIS2_PLACEMENT_3D('',#3170,#2511,#2512) ;
#2075 = AXIS2_PLACEMENT_3D('',#3171,#2513,#2514) ;
#2076 = AXIS2_PLACEMENT_3D('',#3172,#2515,#2516) ;
#2077 = AXIS2_PLACEMENT_3D('',#3173,#2517,#2518) ;
#2078 = AXIS2_PLACEMENT_3D('',#3174,#2519,#2520) ;
#2079 = AXIS2_PLACEMENT_3D('',#3175,#2521,#2522) ;
#2080 = AXIS2_PLACEMENT_3D('',#3176,#2523,#2524) ;
#2081 = AXIS2_PLACEMENT_3D('',#3177,#2525,#2526) ;
#2082 = AXIS2_PLACEMENT_3D('',#3178,#2527,#2528) ;
#2083 = AXIS2_PLACEMENT_3D('',#3179,#2529,#2530) ;
#2084 = AXIS2_PLACEMENT_3D('',#3180,#2531,#2532) ;
#2085 = AXIS2_PLACEMENT_3D('',#3181,#2533,#2534) ;
#2086 = AXIS2_PLACEMENT_3D('',#3182,#2535,#2536) ;
#2087 = AXIS2_PLACEMENT_3D('',#3183,#2537,#2538) ;
#2088 = AXIS2_PLACEMENT_3D('',#3186,#2539,#2540) ;
#2089 = AXIS2_PLACEMENT_3D('',#3188,#2541,#2542) ;
#2090 = AXIS2_PLACEMENT_3D('',#3190,#2543,#2544) ;
#2091 = AXIS2_PLACEMENT_3D('',#3191,#2545,#2546) ;
#2092 = AXIS2_PLACEMENT_3D('',#3192,#2547,#2548) ;
#2093 = AXIS2_PLACEMENT_3D('',#3193,#2549,#2550) ;
#2094 = AXIS2_PLACEMENT_3D('',#3195,#2551,#2552) ;
#2095 = AXIS2_PLACEMENT_3D('',#3198,#2554,#2555) ;
#2096 = AXIS2_PLACEMENT_3D('',#3199,#2556,#2557) ;
#2097 = AXIS2_PLACEMENT_3D('',#3201,#2558,#2559) ;
#2098 = AXIS2_PLACEMENT_3D('',#3203,#2561,#2562) ;
#2099 = AXIS2_PLACEMENT_3D('',#3206,#2564,#2565) ;
#2100 = AXIS2_PLACEMENT_3D('',#3207,#2566,#2567) ;
#2101 = AXIS2_PLACEMENT_3D('',#3208,#2568,#2569) ;
#2102 = AXIS2_PLACEMENT_3D('',#3209,#2570,#2571) ;
#2103 = AXIS2_PLACEMENT_3D('',#3210,#2572,#2573) ;
#2104 = AXIS2_PLACEMENT_3D('',#3212,#2574,#2575) ;
#2105 = AXIS2_PLACEMENT_3D('',#3215,#2577,#2578) ;
#2106 = AXIS2_PLACEMENT_3D('',#3216,#2579,#2580) ;
#2107 = AXIS2_PLACEMENT_3D('',#3218,#2581,#2582) ;
#2108 = AXIS2_PLACEMENT_3D('',#3221,#2584,#2585) ;
#2109 = AXIS2_PLACEMENT_3D('',#3222,#2586,#2587) ;
#2110 = AXIS2_PLACEMENT_3D('',#3223,#2588,#2589) ;
#2111 = AXIS2_PLACEMENT_3D('',#3224,#2590,#2591) ;
#2112 = AXIS2_PLACEMENT_3D('',#3225,#2592,#2593) ;
#2113 = AXIS2_PLACEMENT_3D('',#3226,#2594,#2595) ;
#2114 = AXIS2_PLACEMENT_3D('',#3227,#2596,#2597) ;
#2115 = AXIS2_PLACEMENT_3D('',#3228,#2598,#2599) ;
#2116 = AXIS2_PLACEMENT_3D('',#3229,#2600,#2601) ;
#2117 = AXIS2_PLACEMENT_3D('',#3230,#2602,#2603) ;
#2118 = AXIS2_PLACEMENT_3D('',#3231,#2604,#2605) ;
#2119 = AXIS2_PLACEMENT_3D('',#3232,#2606,#2607) ;
#2120 = AXIS2_PLACEMENT_3D('',#3234,#2608,#2609) ;
#2121 = AXIS2_PLACEMENT_3D('',#3236,#2610,#2611) ;
#2122 = AXIS2_PLACEMENT_3D('',#3237,#2612,#2613) ;
#2123 = AXIS2_PLACEMENT_3D('',#3238,#2614,#2615) ;
#2124 = AXIS2_PLACEMENT_3D('',#3240,#2616,#2617) ;
#2125 = AXIS2_PLACEMENT_3D('',#3242,#2619,#2620) ;
#2126 = AXIS2_PLACEMENT_3D('',#3244,#2621,#2622) ;
#2127 = AXIS2_PLACEMENT_3D('',#3245,#2623,#2624) ;
#2128 = AXIS2_PLACEMENT_3D('',#3246,#2625,#2626) ;
#2129 = AXIS2_PLACEMENT_3D('',#3248,#2627,#2628) ;
#2130 = AXIS2_PLACEMENT_3D('',#3252,#2630,#2631) ;
#2131 = AXIS2_PLACEMENT_3D('',#3253,#2632,#2633) ;
#2132 = AXIS2_PLACEMENT_3D('',#3254,#2634,#2635) ;
#2133 = AXIS2_PLACEMENT_3D('',#3257,#2636,#2637) ;
#2134 = AXIS2_PLACEMENT_3D('',#3258,#2638,#2639) ;
#2135 = AXIS2_PLACEMENT_3D('',#3261,#2641,#2642) ;
#2136 = AXIS2_PLACEMENT_3D('',#3262,#2643,#2644) ;
#2137 = AXIS2_PLACEMENT_3D('',#3265,#2645,#2646) ;
#2138 = AXIS2_PLACEMENT_3D('',#3266,#2647,#2648) ;
#2139 = AXIS2_PLACEMENT_3D('',#3267,#2649,#2650) ;
#2140 = AXIS2_PLACEMENT_3D('',#3268,#2651,#2652) ;
#2141 = AXIS2_PLACEMENT_3D('',#3270,#2653,#2654) ;
#2142 = AXIS2_PLACEMENT_3D('',#3272,#2655,#2656) ;
#2143 = AXIS2_PLACEMENT_3D('',#3273,#2657,#2658) ;
#2144 = AXIS2_PLACEMENT_3D('',#3274,#2659,#2660) ;
#2145 = AXIS2_PLACEMENT_3D('',#3277,#2662,#2663) ;
#2146 = AXIS2_PLACEMENT_3D('',#3278,#2664,#2665) ;
#2147 = AXIS2_PLACEMENT_3D('',#3280,#2666,#2667) ;
#2148 = AXIS2_PLACEMENT_3D('',#3281,#2668,#2669) ;
#2149 = AXIS2_PLACEMENT_3D('',#3282,#2670,#2671) ;
#2150 = AXIS2_PLACEMENT_3D('',#3285,#2673,#2674) ;
#2151 = AXIS2_PLACEMENT_3D('',#3286,#2675,#2676) ;
#2152 = AXIS2_PLACEMENT_3D('',#3288,#2677,#2678) ;
#2153 = AXIS2_PLACEMENT_3D('',#3292,#2680,#2681) ;
#2154 = AXIS2_PLACEMENT_3D('',#3293,#2682,#2683) ;
#2155 = AXIS2_PLACEMENT_3D('',#3294,#2684,#2685) ;
#2156 = AXIS2_PLACEMENT_3D('',#3295,#2686,#2687) ;
#2157 = AXIS2_PLACEMENT_3D('',#3296,#2688,#2689) ;
#2158 = AXIS2_PLACEMENT_3D('',#3297,#2690,#2691) ;
#2159 = AXIS2_PLACEMENT_3D('',#3298,#2692,#2693) ;
#2160 = AXIS2_PLACEMENT_3D('',#3299,#2694,#2695) ;
#2161 = AXIS2_PLACEMENT_3D('',#3300,#2696,#2697) ;
#2162 = AXIS2_PLACEMENT_3D('',#3301,#2698,#2699) ;
#2163 = AXIS2_PLACEMENT_3D('',#3304,#2700,#2701) ;
#2164 = AXIS2_PLACEMENT_3D('',#3305,#2702,#2703) ;
#2165 = AXIS2_PLACEMENT_3D('',#3307,#2704,#2705) ;
#2166 = AXIS2_PLACEMENT_3D('',#3308,#2706,#2707) ;
#2167 = AXIS2_PLACEMENT_3D('',#3309,#2708,#2709) ;
#2168 = AXIS2_PLACEMENT_3D('',#3312,#2710,#2711) ;
#2169 = AXIS2_PLACEMENT_3D('',#3314,#2712,#2713) ;
#2170 = AXIS2_PLACEMENT_3D('',#3316,#2714,#2715) ;
#2171 = AXIS2_PLACEMENT_3D('',#3318,#2716,#2717) ;
#2172 = AXIS2_PLACEMENT_3D('',#3320,#2718,#2719) ;
#2173 = AXIS2_PLACEMENT_3D('',#3321,#2720,#2721) ;
#2174 = AXIS2_PLACEMENT_3D('',#3324,#2723,#2724) ;
#2175 = AXIS2_PLACEMENT_3D('',#3325,#2725,#2726) ;
#2176 = AXIS2_PLACEMENT_3D('',#3327,#2727,#2728) ;
#2177 = AXIS2_PLACEMENT_3D('',#3330,#2730,#2731) ;
#2178 = AXIS2_PLACEMENT_3D('',#3331,#2732,#2733) ;
#2179 = AXIS2_PLACEMENT_3D('',#3333,#2735,#2736) ;
#2180 = AXIS2_PLACEMENT_3D('',#3334,#2737,#2738) ;
#2181 = AXIS2_PLACEMENT_3D('',#3335,#2739,#2740) ;
#2182 = AXIS2_PLACEMENT_3D('',#3339,#2743,#2744) ;
#2183 = AXIS2_PLACEMENT_3D('',#3343,#2747,#2748) ;
#2184 = AXIS2_PLACEMENT_3D('',#3347,#2751,#2752) ;
#2185 = AXIS2_PLACEMENT_3D('',#3351,#2755,#2756) ;
#2186 = AXIS2_PLACEMENT_3D('',#3355,#2759,#2760) ;
#2187 = AXIS2_PLACEMENT_3D('',#3359,#2763,#2764) ;
#2188 = AXIS2_PLACEMENT_3D('',#3362,#2765,#2766) ;
#2189 = AXIS2_PLACEMENT_3D('',#3364,#2767,#2768) ;
#2190 = AXIS2_PLACEMENT_3D('',#3366,#2769,#2770) ;
#2191 = AXIS2_PLACEMENT_3D('',#3368,#2771,#2772) ;
#2192 = AXIS2_PLACEMENT_3D('',#3370,#2773,#2774) ;
#2193 = AXIS2_PLACEMENT_3D('',#3371,#2775,#2776) ;
#2194 = AXIS2_PLACEMENT_3D('',#3372,#2777,#2778) ;
#2195 = AXIS2_PLACEMENT_3D('',#3380,#2779,#2780) ;
#2196 = AXIS2_PLACEMENT_3D('',#3388,#2781,#2782) ;
#2197 = AXIS2_PLACEMENT_3D('',#3396,#2783,#2784) ;
#2198 = AXIS2_PLACEMENT_3D('',#3404,#2785,#2786) ;
#2199 = AXIS2_PLACEMENT_3D('',#3412,#2787,#2788) ;
#2200 = AXIS2_PLACEMENT_3D('',#3420,#2789,#2790) ;
#2201 = AXIS2_PLACEMENT_3D('',#3423,#2793,#2794) ;
#2202 = AXIS2_PLACEMENT_3D('',#3425,#2796,#2797) ;
#2203 = AXIS2_PLACEMENT_3D('',#3427,#2799,#2800) ;
#2204 = AXIS2_PLACEMENT_3D('',#3429,#2802,#2803) ;
#2205 = AXIS2_PLACEMENT_3D('',#3431,#2805,#2806) ;
#2206 = AXIS2_PLACEMENT_3D('',#3432,#2807,#2808) ;
#2207 = AXIS2_PLACEMENT_3D('',#3433,#2809,#2810) ;
#2208 = AXIS2_PLACEMENT_3D('',#3434,#2811,#2812) ;
#2209 = AXIS2_PLACEMENT_3D('',#3435,#2813,#2814) ;
#2210 = AXIS2_PLACEMENT_3D('',#3436,#2815,#2816) ;
#2211 = AXIS2_PLACEMENT_3D('',#3437,#2817,#2818) ;
#2212 = AXIS2_PLACEMENT_3D('',#3438,#2819,#2820) ;
#2213 = AXIS2_PLACEMENT_3D('',#3439,#2821,#2822) ;
#2214 = DIRECTION('axis',(0.,0.,1.)) ;
#2215 = DIRECTION('refdir',(1.,0.,0.)) ;
#2216 = DIRECTION('axis',(0.,0.,1.)) ;
#2217 = DIRECTION('refdir',(1.,0.,0.)) ;
#2218 = DIRECTION('axis',(0.,0.,1.)) ;
#2219 = DIRECTION('refdir',(1.,0.,0.)) ;
#2220 = DIRECTION('center_axis',(-1.,0.,0.)) ;
#2221 = DIRECTION('ref_axis',(0.,0.,1.)) ;
#2222 = DIRECTION('',(0.,-1.,0.)) ;
#2223 = DIRECTION('',(0.,0.,1.)) ;
#2224 = DIRECTION('',(0.,-1.,0.)) ;
#2225 = DIRECTION('',(0.,0.,1.)) ;
#2226 = DIRECTION('center_axis',(-1.21430643318376E-16,1.,0.)) ;
#2227 = DIRECTION('ref_axis',(-1.,-1.21430643318376E-16,0.)) ;
#2228 = DIRECTION('',(-1.,-1.21430643318376E-16,0.)) ;
#2229 = DIRECTION('',(0.,0.,1.)) ;
#2230 = DIRECTION('',(-1.,-1.21430643318376E-16,0.)) ;
#2231 = DIRECTION('center_axis',(1.,0.,0.)) ;
#2232 = DIRECTION('ref_axis',(0.,0.,-1.)) ;
#2233 = DIRECTION('',(0.,1.,0.)) ;
#2234 = DIRECTION('',(0.,0.,1.)) ;
#2235 = DIRECTION('',(0.,1.,0.)) ;
#2236 = DIRECTION('center_axis',(1.21430643318376E-16,-1.,0.)) ;
#2237 = DIRECTION('ref_axis',(1.,1.21430643318376E-16,0.)) ;
#2238 = DIRECTION('',(1.,1.21430643318376E-16,0.)) ;
#2239 = DIRECTION('',(1.,1.21430643318376E-16,0.)) ;
#2240 = DIRECTION('center_axis',(0.,0.,1.)) ;
#2241 = DIRECTION('ref_axis',(1.,0.,0.)) ;
#2242 = DIRECTION('center_axis',(0.,0.,1.)) ;
#2243 = DIRECTION('ref_axis',(1.,0.,0.)) ;
#2244 = DIRECTION('axis',(0.,0.,1.)) ;
#2245 = DIRECTION('refdir',(1.,0.,0.)) ;
#2246 = DIRECTION('center_axis',(0.,0.,-1.)) ;
#2247 = DIRECTION('ref_axis',(-1.,0.,0.)) ;
#2248 = DIRECTION('center_axis',(0.,0.,-1.)) ;
#2249 = DIRECTION('ref_axis',(-1.,0.,0.)) ;
#2250 = DIRECTION('',(0.,0.,-1.)) ;
#2251 = DIRECTION('center_axis',(0.,0.,-1.)) ;
#2252 = DIRECTION('ref_axis',(-1.,0.,0.)) ;
#2253 = DIRECTION('center_axis',(-1.,0.,0.)) ;
#2254 = DIRECTION('ref_axis',(0.,0.,1.)) ;
#2255 = DIRECTION('',(0.,-1.,0.)) ;
#2256 = DIRECTION('',(0.,0.,1.)) ;
#2257 = DIRECTION('',(0.,-1.,0.)) ;
#2258 = DIRECTION('',(0.,0.,1.)) ;
#2259 = DIRECTION('center_axis',(-1.30104260698261E-16,1.,0.)) ;
#2260 = DIRECTION('ref_axis',(-1.,-1.30104260698261E-16,0.)) ;
#2261 = DIRECTION('',(-1.,-1.30104260698261E-16,0.)) ;
#2262 = DIRECTION('',(0.,0.,1.)) ;
#2263 = DIRECTION('',(-1.,-1.30104260698261E-16,0.)) ;
#2264 = DIRECTION('center_axis',(1.,0.,0.)) ;
#2265 = DIRECTION('ref_axis',(0.,0.,-1.)) ;
#2266 = DIRECTION('',(0.,1.,0.)) ;
#2267 = DIRECTION('',(0.,0.,1.)) ;
#2268 = DIRECTION('',(0.,1.,0.)) ;
#2269 = DIRECTION('center_axis',(1.30104260698261E-16,-1.,0.)) ;
#2270 = DIRECTION('ref_axis',(1.,1.30104260698261E-16,0.)) ;
#2271 = DIRECTION('',(1.,1.30104260698261E-16,0.)) ;
#2272 = DIRECTION('',(1.,1.30104260698261E-16,0.)) ;
#2273 = DIRECTION('center_axis',(0.,0.,1.)) ;
#2274 = DIRECTION('ref_axis',(1.,0.,0.)) ;
#2275 = DIRECTION('center_axis',(0.,0.,1.)) ;
#2276 = DIRECTION('ref_axis',(1.,0.,0.)) ;
#2277 = DIRECTION('axis',(0.,0.,1.)) ;
#2278 = DIRECTION('refdir',(1.,0.,0.)) ;
#2279 = DIRECTION('center_axis',(0.,0.,1.)) ;
#2280 = DIRECTION('ref_axis',(1.,0.,0.)) ;
#2281 = DIRECTION('center_axis',(0.,0.,1.)) ;
#2282 = DIRECTION('ref_axis',(1.,0.,0.)) ;
#2283 = DIRECTION('',(0.,0.,1.)) ;
#2284 = DIRECTION('center_axis',(0.,0.,1.)) ;
#2285 = DIRECTION('ref_axis',(1.,0.,0.)) ;
#2286 = DIRECTION('center_axis',(0.,0.,1.)) ;
#2287 = DIRECTION('ref_axis',(1.,0.,0.)) ;
#2288 = DIRECTION('center_axis',(0.,0.,1.)) ;
#2289 = DIRECTION('ref_axis',(1.,0.,0.)) ;
#2290 = DIRECTION('',(0.,0.,1.)) ;
#2291 = DIRECTION('center_axis',(0.,0.,1.)) ;
#2292 = DIRECTION('ref_axis',(-1.,0.,0.)) ;
#2293 = DIRECTION('center_axis',(-2.31296463463574E-16,1.,0.)) ;
#2294 = DIRECTION('ref_axis',(-1.,-2.31296463463574E-16,0.)) ;
#2295 = DIRECTION('',(0.,0.,-1.)) ;
#2296 = DIRECTION('',(-1.,-2.31296463463574E-16,0.)) ;
#2297 = DIRECTION('',(0.,0.,1.)) ;
#2298 = DIRECTION('',(-1.,-2.31296463463574E-16,0.)) ;
#2299 = DIRECTION('center_axis',(1.,0.,0.)) ;
#2300 = DIRECTION('ref_axis',(0.,0.,-1.)) ;
#2301 = DIRECTION('',(0.,1.,0.)) ;
#2302 = DIRECTION('',(0.,0.,1.)) ;
#2303 = DIRECTION('',(0.,1.,0.)) ;
#2304 = DIRECTION('',(0.,0.,1.)) ;
#2305 = DIRECTION('center_axis',(0.,-1.,0.)) ;
#2306 = DIRECTION('ref_axis',(0.,0.,-1.)) ;
#2307 = DIRECTION('',(1.,0.,0.)) ;
#2308 = DIRECTION('',(0.,0.,1.)) ;
#2309 = DIRECTION('',(1.,0.,0.)) ;
#2310 = DIRECTION('center_axis',(-1.,0.,0.)) ;
#2311 = DIRECTION('ref_axis',(0.,0.,1.)) ;
#2312 = DIRECTION('',(0.,-1.,0.)) ;
#2313 = DIRECTION('',(0.,0.,1.)) ;
#2314 = DIRECTION('',(0.,-1.,0.)) ;
#2315 = DIRECTION('center_axis',(-0.882352941176471,0.470588235294118,0.)) ;
#2316 = DIRECTION('ref_axis',(-0.470588235294118,-0.882352941176471,0.)) ;
#2317 = DIRECTION('',(-0.470588235294118,-0.88235294117647,0.)) ;
#2318 = DIRECTION('',(0.,0.,1.)) ;
#2319 = DIRECTION('',(-0.470588235294118,-0.88235294117647,0.)) ;
#2320 = DIRECTION('center_axis',(-2.31296463463574E-16,1.,0.)) ;
#2321 = DIRECTION('ref_axis',(-1.,-2.31296463463574E-16,0.)) ;
#2322 = DIRECTION('',(0.,0.,1.)) ;
#2323 = DIRECTION('',(-1.,-2.31296463463574E-16,0.)) ;
#2324 = DIRECTION('',(-1.,-2.31296463463574E-16,0.)) ;
#2325 = DIRECTION('center_axis',(0.882352941176471,0.470588235294118,0.)) ;
#2326 = DIRECTION('ref_axis',(-0.470588235294118,0.882352941176471,0.)) ;
#2327 = DIRECTION('',(-0.470588235294118,0.882352941176471,0.)) ;
#2328 = DIRECTION('',(-0.470588235294118,0.882352941176471,0.)) ;
#2329 = DIRECTION('center_axis',(0.,0.,1.)) ;
#2330 = DIRECTION('ref_axis',(1.,0.,0.)) ;
#2331 = DIRECTION('',(1.,0.,0.)) ;
#2332 = DIRECTION('',(0.,1.,0.)) ;
#2333 = DIRECTION('',(9.25185853854297E-17,-1.,0.)) ;
#2334 = DIRECTION('center_axis',(0.,0.,1.)) ;
#2335 = DIRECTION('ref_axis',(1.,0.,0.)) ;
#2336 = DIRECTION('',(0.,1.,0.)) ;
#2337 = DIRECTION('',(1.,0.,0.)) ;
#2338 = DIRECTION('',(9.25185853854297E-17,-1.,0.)) ;
#2339 = DIRECTION('center_axis',(0.,-1.,0.)) ;
#2340 = DIRECTION('ref_axis',(0.,0.,-1.)) ;
#2341 = DIRECTION('',(0.,0.,1.)) ;
#2342 = DIRECTION('',(0.,0.,1.)) ;
#2343 = DIRECTION('center_axis',(1.,0.,0.)) ;
#2344 = DIRECTION('ref_axis',(0.,0.,-1.)) ;
#2345 = DIRECTION('center_axis',(-1.,-9.25185853854297E-17,0.)) ;
#2346 = DIRECTION('ref_axis',(9.25185853854297E-17,-1.,0.)) ;
#2347 = DIRECTION('',(0.,0.,1.)) ;
#2348 = DIRECTION('',(1.,0.,0.)) ;
#2349 = DIRECTION('',(-3.49148133884326E-15,-1.,-2.09488880330588E-14)) ;
#2350 = DIRECTION('',(1.,-3.49148133884297E-15,-1.39659253553725E-14)) ;
#2351 = DIRECTION('',(0.,-1.,-3.49148133884313E-15)) ;
#2352 = DIRECTION('',(1.,0.,0.)) ;
#2353 = DIRECTION('',(0.,0.,1.)) ;
#2354 = DIRECTION('',(1.,0.,0.)) ;
#2355 = DIRECTION('axis',(0.,0.,1.)) ;
#2356 = DIRECTION('refdir',(1.,0.,0.)) ;
#2357 = DIRECTION('axis',(0.,0.,1.)) ;
#2358 = DIRECTION('refdir',(1.,0.,0.)) ;
#2359 = DIRECTION('center_axis',(0.,1.,0.)) ;
#2360 = DIRECTION('ref_axis',(0.,0.,1.)) ;
#2361 = DIRECTION('',(0.,1.,0.)) ;
#2362 = DIRECTION('center_axis',(1.,2.84764536702765E-17,0.)) ;
#2363 = DIRECTION('ref_axis',(-2.84764536702765E-17,1.,0.)) ;
#2364 = DIRECTION('center_axis',(1.,2.84764536702765E-17,0.)) ;
#2365 = DIRECTION('ref_axis',(2.84764536702765E-17,-1.,0.)) ;
#2366 = DIRECTION('',(-0.707106781186551,0.707106781186544,8.65956056235489E-17)) ;
#2367 = DIRECTION('center_axis',(-1.,-2.84764536702765E-17,0.)) ;
#2368 = DIRECTION('ref_axis',(-2.84764536702765E-17,1.,0.)) ;
#2369 = DIRECTION('center_axis',(1.,2.84764536702764E-17,0.)) ;
#2370 = DIRECTION('ref_axis',(-2.84764536702764E-17,1.,0.)) ;
#2371 = DIRECTION('center_axis',(1.,2.84764536702764E-17,0.)) ;
#2372 = DIRECTION('ref_axis',(-2.84764536702764E-17,1.,0.)) ;
#2373 = DIRECTION('',(-1.,-2.84764536702764E-17,0.)) ;
#2374 = DIRECTION('',(-1.,-2.84764536702764E-17,0.)) ;
#2375 = DIRECTION('center_axis',(1.,2.84764536702764E-17,0.)) ;
#2376 = DIRECTION('ref_axis',(-2.84764536702764E-17,1.,0.)) ;
#2377 = DIRECTION('',(-1.,-2.84764536702764E-17,0.)) ;
#2378 = DIRECTION('center_axis',(1.,2.84764536702764E-17,0.)) ;
#2379 = DIRECTION('ref_axis',(-2.84764536702764E-17,1.,0.)) ;
#2380 = DIRECTION('center_axis',(-1.,-2.84764536702764E-17,0.)) ;
#2381 = DIRECTION('ref_axis',(2.84764536702764E-17,-1.,0.)) ;
#2382 = DIRECTION('center_axis',(1.,2.84764536702764E-17,0.)) ;
#2383 = DIRECTION('ref_axis',(-2.84764536702764E-17,1.,0.)) ;
#2384 = DIRECTION('axis',(0.,0.,1.)) ;
#2385 = DIRECTION('refdir',(1.,0.,0.)) ;
#2386 = DIRECTION('center_axis',(0.,0.,-1.)) ;
#2387 = DIRECTION('ref_axis',(-1.,0.,0.)) ;
#2388 = DIRECTION('center_axis',(0.,0.,1.)) ;
#2389 = DIRECTION('ref_axis',(1.,0.,0.)) ;
#2390 = DIRECTION('',(0.,0.,1.)) ;
#2391 = DIRECTION('center_axis',(0.,0.,1.)) ;
#2392 = DIRECTION('ref_axis',(1.,0.,0.)) ;
#2393 = DIRECTION('center_axis',(0.,0.,1.)) ;
#2394 = DIRECTION('ref_axis',(1.,0.,0.)) ;
#2395 = DIRECTION('center_axis',(0.,0.,1.)) ;
#2396 = DIRECTION('ref_axis',(1.,0.,0.)) ;
#2397 = DIRECTION('axis',(0.,0.,1.)) ;
#2398 = DIRECTION('refdir',(1.,0.,0.)) ;
#2399 = DIRECTION('center_axis',(1.,0.,0.)) ;
#2400 = DIRECTION('ref_axis',(0.,0.,-1.)) ;
#2401 = DIRECTION('center_axis',(1.,0.,0.)) ;
#2402 = DIRECTION('ref_axis',(0.,0.,-1.)) ;
#2403 = DIRECTION('',(1.,0.,0.)) ;
#2404 = DIRECTION('center_axis',(1.,0.,0.)) ;
#2405 = DIRECTION('ref_axis',(0.,0.,-1.)) ;
#2406 = DIRECTION('center_axis',(0.,1.,0.)) ;
#2407 = DIRECTION('ref_axis',(0.,0.,1.)) ;
#2408 = DIRECTION('center_axis',(0.,1.,0.)) ;
#2409 = DIRECTION('ref_axis',(0.,0.,1.)) ;
#2410 = DIRECTION('',(0.,1.,0.)) ;
#2411 = DIRECTION('center_axis',(0.,1.,0.)) ;
#2412 = DIRECTION('ref_axis',(0.,0.,1.)) ;
#2413 = DIRECTION('center_axis',(1.,0.,0.)) ;
#2414 = DIRECTION('ref_axis',(0.,0.,-1.)) ;
#2415 = DIRECTION('',(0.,-1.,0.)) ;
#2416 = DIRECTION('',(0.,0.,-1.)) ;
#2417 = DIRECTION('',(0.,-1.,0.)) ;
#2418 = DIRECTION('',(0.,0.,-1.)) ;
#2419 = DIRECTION('center_axis',(0.,1.,0.)) ;
#2420 = DIRECTION('ref_axis',(0.,0.,1.)) ;
#2421 = DIRECTION('',(1.,0.,0.)) ;
#2422 = DIRECTION('',(0.,0.,-1.)) ;
#2423 = DIRECTION('',(1.,0.,0.)) ;
#2424 = DIRECTION('center_axis',(-1.,0.,0.)) ;
#2425 = DIRECTION('ref_axis',(0.,0.,1.)) ;
#2426 = DIRECTION('',(0.,1.,0.)) ;
#2427 = DIRECTION('',(0.,0.,-1.)) ;
#2428 = DIRECTION('',(0.,1.,0.)) ;
#2429 = DIRECTION('center_axis',(0.,-1.,0.)) ;
#2430 = DIRECTION('ref_axis',(0.,0.,-1.)) ;
#2431 = DIRECTION('',(-1.,0.,0.)) ;
#2432 = DIRECTION('',(-1.,0.,0.)) ;
#2433 = DIRECTION('center_axis',(0.,0.,1.)) ;
#2434 = DIRECTION('ref_axis',(1.,0.,0.)) ;
#2435 = DIRECTION('center_axis',(0.,0.,1.)) ;
#2436 = DIRECTION('ref_axis',(1.,0.,0.)) ;
#2437 = DIRECTION('center_axis',(0.,1.,0.)) ;
#2438 = DIRECTION('ref_axis',(0.,0.,1.)) ;
#2439 = DIRECTION('axis',(0.,0.,1.)) ;
#2440 = DIRECTION('refdir',(1.,0.,0.)) ;
#2441 = DIRECTION('center_axis',(1.,0.,0.)) ;
#2442 = DIRECTION('ref_axis',(0.,0.,-1.)) ;
#2443 = DIRECTION('center_axis',(1.,0.,0.)) ;
#2444 = DIRECTION('ref_axis',(0.,0.,-1.)) ;
#2445 = DIRECTION('',(1.,0.,0.)) ;
#2446 = DIRECTION('center_axis',(1.,0.,0.)) ;
#2447 = DIRECTION('ref_axis',(0.,0.,-1.)) ;
#2448 = DIRECTION('center_axis',(1.,0.,0.)) ;
#2449 = DIRECTION('ref_axis',(0.,0.,-1.)) ;
#2450 = DIRECTION('',(0.515038074910058,-1.04972719113862E-16,0.85716730070211)) ;
#2451 = DIRECTION('center_axis',(1.,0.,0.)) ;
#2452 = DIRECTION('ref_axis',(0.,0.,-1.)) ;
#2453 = DIRECTION('center_axis',(1.,0.,0.)) ;
#2454 = DIRECTION('ref_axis',(0.,0.,-1.)) ;
#2455 = DIRECTION('',(-1.,0.,0.)) ;
#2456 = DIRECTION('center_axis',(1.,0.,0.)) ;
#2457 = DIRECTION('ref_axis',(0.,0.,-1.)) ;
#2458 = DIRECTION('center_axis',(1.,0.,0.)) ;
#2459 = DIRECTION('ref_axis',(0.,0.,-1.)) ;
#2460 = DIRECTION('center_axis',(1.,0.,0.)) ;
#2461 = DIRECTION('ref_axis',(0.,0.,-1.)) ;
#2462 = DIRECTION('',(-1.,0.,0.)) ;
#2463 = DIRECTION('center_axis',(1.,0.,0.)) ;
#2464 = DIRECTION('ref_axis',(0.,0.,-1.)) ;
#2465 = DIRECTION('center_axis',(1.,0.,0.)) ;
#2466 = DIRECTION('ref_axis',(0.,0.,-1.)) ;
#2467 = DIRECTION('center_axis',(1.,0.,0.)) ;
#2468 = DIRECTION('ref_axis',(0.,0.,-1.)) ;
#2469 = DIRECTION('',(-1.,0.,0.)) ;
#2470 = DIRECTION('center_axis',(1.,0.,0.)) ;
#2471 = DIRECTION('ref_axis',(0.,0.,-1.)) ;
#2472 = DIRECTION('center_axis',(-1.,0.,0.)) ;
#2473 = DIRECTION('ref_axis',(0.,0.,1.)) ;
#2474 = DIRECTION('center_axis',(1.,0.,0.)) ;
#2475 = DIRECTION('ref_axis',(0.,0.,-1.)) ;
#2476 = DIRECTION('center_axis',(1.,0.,0.)) ;
#2477 = DIRECTION('ref_axis',(0.,0.,-1.)) ;
#2478 = DIRECTION('center_axis',(1.,0.,0.)) ;
#2479 = DIRECTION('ref_axis',(0.,0.,-1.)) ;
#2480 = DIRECTION('axis',(0.,0.,1.)) ;
#2481 = DIRECTION('refdir',(1.,0.,0.)) ;
#2482 = DIRECTION('center_axis',(1.,0.,0.)) ;
#2483 = DIRECTION('ref_axis',(0.,0.,-1.)) ;
#2484 = DIRECTION('center_axis',(1.,0.,0.)) ;
#2485 = DIRECTION('ref_axis',(0.,0.,-1.)) ;
#2486 = DIRECTION('',(1.,0.,0.)) ;
#2487 = DIRECTION('center_axis',(1.,0.,0.)) ;
#2488 = DIRECTION('ref_axis',(0.,0.,-1.)) ;
#2489 = DIRECTION('center_axis',(1.,0.,0.)) ;
#2490 = DIRECTION('ref_axis',(0.,0.,-1.)) ;
#2491 = DIRECTION('',(0.515038074910058,-1.04972719113862E-16,0.85716730070211)) ;
#2492 = DIRECTION('center_axis',(1.,-1.18008399726313E-17,0.)) ;
#2493 = DIRECTION('ref_axis',(1.18008399726313E-17,1.,0.)) ;
#2494 = DIRECTION('center_axis',(1.,-1.18008399726313E-17,0.)) ;
#2495 = DIRECTION('ref_axis',(1.18008399726313E-17,1.,0.)) ;
#2496 = DIRECTION('',(-1.,1.18008399726313E-17,0.)) ;
#2497 = DIRECTION('center_axis',(1.,-1.18008399726313E-17,0.)) ;
#2498 = DIRECTION('ref_axis',(1.18008399726313E-17,1.,0.)) ;
#2499 = DIRECTION('center_axis',(1.,-1.18008399726313E-17,0.)) ;
#2500 = DIRECTION('ref_axis',(1.18008399726313E-17,1.,0.)) ;
#2501 = DIRECTION('center_axis',(1.,-1.18008399726313E-17,0.)) ;
#2502 = DIRECTION('ref_axis',(1.18008399726313E-17,1.,0.)) ;
#2503 = DIRECTION('',(-1.,1.18008399726313E-17,0.)) ;
#2504 = DIRECTION('center_axis',(1.,-1.18008399726313E-17,0.)) ;
#2505 = DIRECTION('ref_axis',(1.18008399726313E-17,1.,0.)) ;
#2506 = DIRECTION('center_axis',(1.,-1.18008399726313E-17,0.)) ;
#2507 = DIRECTION('ref_axis',(1.18008399726313E-17,1.,0.)) ;
#2508 = DIRECTION('center_axis',(1.,-1.18008399726313E-17,0.)) ;
#2509 = DIRECTION('ref_axis',(1.18008399726313E-17,1.,0.)) ;
#2510 = DIRECTION('',(-1.,1.18008399726313E-17,0.)) ;
#2511 = DIRECTION('center_axis',(1.,-1.18008399726313E-17,0.)) ;
#2512 = DIRECTION('ref_axis',(1.18008399726313E-17,1.,0.)) ;
#2513 = DIRECTION('center_axis',(-1.,1.18008399726313E-17,0.)) ;
#2514 = DIRECTION('ref_axis',(-1.18008399726313E-17,-1.,0.)) ;
#2515 = DIRECTION('center_axis',(1.,-1.18008399726313E-17,0.)) ;
#2516 = DIRECTION('ref_axis',(1.18008399726313E-17,1.,0.)) ;
#2517 = DIRECTION('center_axis',(1.,-1.18008399726313E-17,0.)) ;
#2518 = DIRECTION('ref_axis',(1.18008399726313E-17,1.,0.)) ;
#2519 = DIRECTION('center_axis',(1.,-1.18008399726313E-17,0.)) ;
#2520 = DIRECTION('ref_axis',(1.18008399726313E-17,1.,0.)) ;
#2521 = DIRECTION('',(-0.280405930446127,-6.93889390388847E-16,0.959881510484832)) ;
#2522 = DIRECTION('',(-1.35458620979689E-16,1.,6.833197457932E-16)) ;
#2523 = DIRECTION('',(-0.959881510484832,-2.20628314263265E-16,-0.280405930446127)) ;
#2524 = DIRECTION('',(0.0684984195870195,0.969703967768755,-0.234482795547167)) ;
#2525 = DIRECTION('',(1.,9.75235355159187E-29,-3.49148133884313E-15)) ;
#2526 = DIRECTION('',(-3.49148133884313E-15,2.79318507107451E-14,-1.)) ;
#2527 = DIRECTION('',(-0.936484761020976,-0.350708272465144,-3.94520260830031E-17)) ;
#2528 = DIRECTION('',(5.75649883131134E-17,-2.66206325132702E-16,1.)) ;
#2529 = DIRECTION('',(3.49148133884316E-15,1.,3.49148133884311E-15)) ;
#2530 = DIRECTION('',(6.98296267768625E-15,-3.49148133884313E-15,1.)) ;
#2531 = DIRECTION('',(3.49148133884316E-15,1.,3.49148133884311E-15)) ;
#2532 = DIRECTION('',(6.98296267768625E-15,-3.49148133884313E-15,1.)) ;
#2533 = DIRECTION('axis',(0.,0.,1.)) ;
#2534 = DIRECTION('refdir',(1.,0.,0.)) ;
#2535 = DIRECTION('axis',(0.,0.,1.)) ;
#2536 = DIRECTION('refdir',(1.,0.,0.)) ;
#2537 = DIRECTION('center_axis',(0.,0.,1.)) ;
#2538 = DIRECTION('ref_axis',(1.,0.,0.)) ;
#2539 = DIRECTION('center_axis',(0.,0.,-1.)) ;
#2540 = DIRECTION('ref_axis',(-1.,0.,0.)) ;
#2541 = DIRECTION('center_axis',(-1.22464679914735E-16,1.,0.)) ;
#2542 = DIRECTION('ref_axis',(-1.,-1.22464679914735E-16,0.)) ;
#2543 = DIRECTION('center_axis',(0.,0.,1.)) ;
#2544 = DIRECTION('ref_axis',(1.,0.,0.)) ;
#2545 = DIRECTION('center_axis',(0.,0.,1.)) ;
#2546 = DIRECTION('ref_axis',(1.,0.,0.)) ;
#2547 = DIRECTION('center_axis',(0.,0.,-1.)) ;
#2548 = DIRECTION('ref_axis',(-1.,0.,0.)) ;
#2549 = DIRECTION('center_axis',(0.,0.,1.)) ;
#2550 = DIRECTION('ref_axis',(1.,0.,0.)) ;
#2551 = DIRECTION('center_axis',(0.,0.,1.)) ;
#2552 = DIRECTION('ref_axis',(1.,0.,0.)) ;
#2553 = DIRECTION('',(0.,0.,1.)) ;
#2554 = DIRECTION('center_axis',(0.,0.,1.)) ;
#2555 = DIRECTION('ref_axis',(1.,0.,0.)) ;
#2556 = DIRECTION('center_axis',(0.,0.,-1.)) ;
#2557 = DIRECTION('ref_axis',(-1.,0.,0.)) ;
#2558 = DIRECTION('center_axis',(0.,0.,1.)) ;
#2559 = DIRECTION('ref_axis',(1.,0.,0.)) ;
#2560 = DIRECTION('',(0.,0.,1.)) ;
#2561 = DIRECTION('center_axis',(0.,0.,-1.)) ;
#2562 = DIRECTION('ref_axis',(-1.,0.,0.)) ;
#2563 = DIRECTION('',(0.,0.,1.)) ;
#2564 = DIRECTION('center_axis',(0.,0.,1.)) ;
#2565 = DIRECTION('ref_axis',(1.,0.,0.)) ;
#2566 = DIRECTION('center_axis',(0.,0.,1.)) ;
#2567 = DIRECTION('ref_axis',(1.,0.,0.)) ;
#2568 = DIRECTION('center_axis',(0.,0.,1.)) ;
#2569 = DIRECTION('ref_axis',(1.,0.,0.)) ;
#2570 = DIRECTION('axis',(0.,0.,1.)) ;
#2571 = DIRECTION('refdir',(1.,0.,0.)) ;
#2572 = DIRECTION('center_axis',(-1.,0.,0.)) ;
#2573 = DIRECTION('ref_axis',(0.,0.,1.)) ;
#2574 = DIRECTION('center_axis',(1.,0.,0.)) ;
#2575 = DIRECTION('ref_axis',(0.,0.,-1.)) ;
#2576 = DIRECTION('',(-1.,0.,0.)) ;
#2577 = DIRECTION('center_axis',(1.,0.,0.)) ;
#2578 = DIRECTION('ref_axis',(0.,0.,-1.)) ;
#2579 = DIRECTION('center_axis',(-1.,0.,0.)) ;
#2580 = DIRECTION('ref_axis',(0.,0.,1.)) ;
#2581 = DIRECTION('center_axis',(1.,0.,0.)) ;
#2582 = DIRECTION('ref_axis',(0.,0.,-1.)) ;
#2583 = DIRECTION('',(1.,0.,0.)) ;
#2584 = DIRECTION('center_axis',(1.,0.,0.)) ;
#2585 = DIRECTION('ref_axis',(0.,0.,-1.)) ;
#2586 = DIRECTION('center_axis',(1.,0.,0.)) ;
#2587 = DIRECTION('ref_axis',(0.,0.,-1.)) ;
#2588 = DIRECTION('center_axis',(1.,0.,0.)) ;
#2589 = DIRECTION('ref_axis',(0.,0.,-1.)) ;
#2590 = DIRECTION('',(0.,0.,1.)) ;
#2591 = DIRECTION('',(0.981078544696235,-0.193610147297907,0.)) ;
#2592 = DIRECTION('',(-0.622561358902543,-0.782570990007564,1.67852253791786E-30)) ;
#2593 = DIRECTION('',(-1.04498327215469E-30,-1.31356304424839E-30,-1.)) ;
#2594 = DIRECTION('',(0.,0.,1.)) ;
#2595 = DIRECTION('',(0.981078544696235,-0.193610147297907,0.)) ;
#2596 = DIRECTION('',(0.,0.,1.)) ;
#2597 = DIRECTION('',(0.981078544696235,-0.193610147297907,0.)) ;
#2598 = DIRECTION('',(0.545029383677348,0.838416943369044,0.)) ;
#2599 = DIRECTION('',(0.,0.,1.)) ;
#2600 = DIRECTION('',(-0.30739286847475,-0.95158269446794,0.)) ;
#2601 = DIRECTION('',(0.,0.,-1.)) ;
#2602 = DIRECTION('axis',(0.,0.,1.)) ;
#2603 = DIRECTION('refdir',(1.,0.,0.)) ;
#2604 = DIRECTION('axis',(0.,0.,1.)) ;
#2605 = DIRECTION('refdir',(1.,0.,0.)) ;
#2606 = DIRECTION('center_axis',(1.,0.,0.)) ;
#2607 = DIRECTION('ref_axis',(0.,0.,-1.)) ;
#2608 = DIRECTION('center_axis',(1.,0.,0.)) ;
#2609 = DIRECTION('ref_axis',(0.,0.,-1.)) ;
#2610 = DIRECTION('center_axis',(0.,-1.,-1.22464679914735E-16)) ;
#2611 = DIRECTION('ref_axis',(0.,-1.22464679914735E-16,1.)) ;
#2612 = DIRECTION('center_axis',(1.,0.,0.)) ;
#2613 = DIRECTION('ref_axis',(0.,0.,-1.)) ;
#2614 = DIRECTION('center_axis',(1.,0.,0.)) ;
#2615 = DIRECTION('ref_axis',(0.,0.,-1.)) ;
#2616 = DIRECTION('center_axis',(1.,0.,0.)) ;
#2617 = DIRECTION('ref_axis',(0.,0.,-1.)) ;
#2618 = DIRECTION('',(-1.,0.,0.)) ;
#2619 = DIRECTION('center_axis',(1.,0.,0.)) ;
#2620 = DIRECTION('ref_axis',(0.,0.,-1.)) ;
#2621 = DIRECTION('center_axis',(1.,0.,0.)) ;
#2622 = DIRECTION('ref_axis',(0.,0.,-1.)) ;
#2623 = DIRECTION('center_axis',(0.,-1.,-1.22464679914735E-16)) ;
#2624 = DIRECTION('ref_axis',(0.,-1.22464679914735E-16,1.)) ;
#2625 = DIRECTION('center_axis',(1.,0.,0.)) ;
#2626 = DIRECTION('ref_axis',(0.,0.,-1.)) ;
#2627 = DIRECTION('center_axis',(1.,0.,0.)) ;
#2628 = DIRECTION('ref_axis',(0.,0.,-1.)) ;
#2629 = DIRECTION('',(1.,0.,0.)) ;
#2630 = DIRECTION('center_axis',(-1.,0.,0.)) ;
#2631 = DIRECTION('ref_axis',(0.,0.,-1.)) ;
#2632 = DIRECTION('center_axis',(-1.,0.,0.)) ;
#2633 = DIRECTION('ref_axis',(0.,0.,-1.)) ;
#2634 = DIRECTION('center_axis',(1.,0.,0.)) ;
#2635 = DIRECTION('ref_axis',(0.,0.,-1.)) ;
#2636 = DIRECTION('center_axis',(1.,0.,0.)) ;
#2637 = DIRECTION('ref_axis',(0.,0.,1.)) ;
#2638 = DIRECTION('center_axis',(1.,0.,0.)) ;
#2639 = DIRECTION('ref_axis',(0.,0.,1.)) ;
#2640 = DIRECTION('',(1.,0.,0.)) ;
#2641 = DIRECTION('center_axis',(1.,0.,0.)) ;
#2642 = DIRECTION('ref_axis',(0.,0.,-1.)) ;
#2643 = DIRECTION('center_axis',(-1.,0.,0.)) ;
#2644 = DIRECTION('ref_axis',(0.,0.,1.)) ;
#2645 = DIRECTION('center_axis',(1.,0.,0.)) ;
#2646 = DIRECTION('ref_axis',(0.,0.,-1.)) ;
#2647 = DIRECTION('center_axis',(0.,-1.,1.22464679914735E-16)) ;
#2648 = DIRECTION('ref_axis',(0.,-1.22464679914735E-16,-1.)) ;
#2649 = DIRECTION('center_axis',(1.,0.,0.)) ;
#2650 = DIRECTION('ref_axis',(0.,0.,-1.)) ;
#2651 = DIRECTION('center_axis',(1.,0.,0.)) ;
#2652 = DIRECTION('ref_axis',(0.,0.,-1.)) ;
#2653 = DIRECTION('center_axis',(1.,0.,0.)) ;
#2654 = DIRECTION('ref_axis',(0.,0.,-1.)) ;
#2655 = DIRECTION('center_axis',(0.,-1.,-1.22464679914735E-16)) ;
#2656 = DIRECTION('ref_axis',(0.,-1.22464679914735E-16,1.)) ;
#2657 = DIRECTION('center_axis',(1.,0.,0.)) ;
#2658 = DIRECTION('ref_axis',(0.,0.,-1.)) ;
#2659 = DIRECTION('center_axis',(1.,0.,0.)) ;
#2660 = DIRECTION('ref_axis',(0.,0.,-1.)) ;
#2661 = DIRECTION('',(1.,0.,0.)) ;
#2662 = DIRECTION('center_axis',(1.,0.,0.)) ;
#2663 = DIRECTION('ref_axis',(0.,0.,-1.)) ;
#2664 = DIRECTION('center_axis',(1.,0.,0.)) ;
#2665 = DIRECTION('ref_axis',(0.,0.,-1.)) ;
#2666 = DIRECTION('center_axis',(0.,-1.,-1.22464679914735E-16)) ;
#2667 = DIRECTION('ref_axis',(0.,-1.22464679914735E-16,1.)) ;
#2668 = DIRECTION('center_axis',(1.,0.,0.)) ;
#2669 = DIRECTION('ref_axis',(0.,0.,-1.)) ;
#2670 = DIRECTION('center_axis',(1.,0.,0.)) ;
#2671 = DIRECTION('ref_axis',(0.,0.,-1.)) ;
#2672 = DIRECTION('',(-1.,0.,0.)) ;
#2673 = DIRECTION('center_axis',(1.,0.,0.)) ;
#2674 = DIRECTION('ref_axis',(0.,0.,-1.)) ;
#2675 = DIRECTION('center_axis',(1.,0.,0.)) ;
#2676 = DIRECTION('ref_axis',(0.,0.,-1.)) ;
#2677 = DIRECTION('center_axis',(1.,0.,0.)) ;
#2678 = DIRECTION('ref_axis',(0.,0.,-1.)) ;
#2679 = DIRECTION('',(-1.,0.,0.)) ;
#2680 = DIRECTION('center_axis',(-1.,0.,0.)) ;
#2681 = DIRECTION('ref_axis',(0.,0.,1.)) ;
#2682 = DIRECTION('center_axis',(-1.,0.,0.)) ;
#2683 = DIRECTION('ref_axis',(0.,0.,1.)) ;
#2684 = DIRECTION('center_axis',(-1.,0.,0.)) ;
#2685 = DIRECTION('ref_axis',(0.,0.,1.)) ;
#2686 = DIRECTION('center_axis',(0.,-1.,1.22464679914735E-16)) ;
#2687 = DIRECTION('ref_axis',(0.,-1.22464679914735E-16,-1.)) ;
#2688 = DIRECTION('center_axis',(1.,0.,0.)) ;
#2689 = DIRECTION('ref_axis',(0.,0.,-1.)) ;
#2690 = DIRECTION('center_axis',(-1.,0.,0.)) ;
#2691 = DIRECTION('ref_axis',(0.,0.,1.)) ;
#2692 = DIRECTION('center_axis',(1.,0.,0.)) ;
#2693 = DIRECTION('ref_axis',(0.,0.,-1.)) ;
#2694 = DIRECTION('center_axis',(-1.,0.,0.)) ;
#2695 = DIRECTION('ref_axis',(0.,0.,1.)) ;
#2696 = DIRECTION('axis',(0.,0.,1.)) ;
#2697 = DIRECTION('refdir',(1.,0.,0.)) ;
#2698 = DIRECTION('center_axis',(1.,0.,0.)) ;
#2699 = DIRECTION('ref_axis',(0.,0.,-1.)) ;
#2700 = DIRECTION('center_axis',(1.,0.,0.)) ;
#2701 = DIRECTION('ref_axis',(0.,0.,-1.)) ;
#2702 = DIRECTION('center_axis',(1.,0.,0.)) ;
#2703 = DIRECTION('ref_axis',(0.,0.,-1.)) ;
#2704 = DIRECTION('center_axis',(0.,1.,1.22464679914735E-16)) ;
#2705 = DIRECTION('ref_axis',(0.,-1.22464679914735E-16,1.)) ;
#2706 = DIRECTION('center_axis',(-1.,0.,0.)) ;
#2707 = DIRECTION('ref_axis',(0.,0.,-1.)) ;
#2708 = DIRECTION('center_axis',(-1.,0.,0.)) ;
#2709 = DIRECTION('ref_axis',(0.,0.,1.)) ;
#2710 = DIRECTION('center_axis',(-1.,0.,0.)) ;
#2711 = DIRECTION('ref_axis',(0.,0.,1.)) ;
#2712 = DIRECTION('center_axis',(-1.,0.,0.)) ;
#2713 = DIRECTION('ref_axis',(0.,0.,1.)) ;
#2714 = DIRECTION('center_axis',(-1.,0.,0.)) ;
#2715 = DIRECTION('ref_axis',(0.,0.,1.)) ;
#2716 = DIRECTION('center_axis',(-1.,0.,0.)) ;
#2717 = DIRECTION('ref_axis',(0.,0.,1.)) ;
#2718 = DIRECTION('center_axis',(-1.,0.,0.)) ;
#2719 = DIRECTION('ref_axis',(0.,0.,1.)) ;
#2720 = DIRECTION('center_axis',(-1.,0.,0.)) ;
#2721 = DIRECTION('ref_axis',(0.,0.,1.)) ;
#2722 = DIRECTION('',(1.,0.,0.)) ;
#2723 = DIRECTION('center_axis',(1.,0.,0.)) ;
#2724 = DIRECTION('ref_axis',(0.,0.,-1.)) ;
#2725 = DIRECTION('center_axis',(-1.,0.,0.)) ;
#2726 = DIRECTION('ref_axis',(0.,0.,1.)) ;
#2727 = DIRECTION('center_axis',(-1.,0.,0.)) ;
#2728 = DIRECTION('ref_axis',(0.,0.,1.)) ;
#2729 = DIRECTION('',(0.707106781186553,8.65956056235487E-17,0.707106781186542)) ;
#2730 = DIRECTION('center_axis',(-1.,0.,0.)) ;
#2731 = DIRECTION('ref_axis',(0.,0.,1.)) ;
#2732 = DIRECTION('center_axis',(-1.,0.,0.)) ;
#2733 = DIRECTION('ref_axis',(0.,0.,1.)) ;
#2734 = DIRECTION('',(1.,0.,0.)) ;
#2735 = DIRECTION('center_axis',(1.,0.,0.)) ;
#2736 = DIRECTION('ref_axis',(0.,0.,-1.)) ;
#2737 = DIRECTION('center_axis',(-1.,0.,0.)) ;
#2738 = DIRECTION('ref_axis',(0.,0.,1.)) ;
#2739 = DIRECTION('center_axis',(1.,0.,0.)) ;
#2740 = DIRECTION('ref_axis',(0.,0.,-1.)) ;
#2741 = DIRECTION('',(0.,0.500000000000002,0.866025403784438)) ;
#2742 = DIRECTION('',(0.,1.,2.3112532288264E-16)) ;
#2743 = DIRECTION('center_axis',(1.,0.,0.)) ;
#2744 = DIRECTION('ref_axis',(0.,0.,-1.)) ;
#2745 = DIRECTION('',(0.,0.500000000000002,0.866025403784438)) ;
#2746 = DIRECTION('',(0.,-0.5,0.866025403784438)) ;
#2747 = DIRECTION('center_axis',(1.,0.,0.)) ;
#2748 = DIRECTION('ref_axis',(0.,0.,-1.)) ;
#2749 = DIRECTION('',(0.,-0.5,0.866025403784438)) ;
#2750 = DIRECTION('',(0.,-1.,2.3112532288264E-16)) ;
#2751 = DIRECTION('center_axis',(1.,0.,0.)) ;
#2752 = DIRECTION('ref_axis',(0.,0.,-1.)) ;
#2753 = DIRECTION('',(0.,-1.,2.3112532288264E-16)) ;
#2754 = DIRECTION('',(0.,-0.500000000000002,-0.866025403784438)) ;
#2755 = DIRECTION('center_axis',(1.,0.,0.)) ;
#2756 = DIRECTION('ref_axis',(0.,0.,-1.)) ;
#2757 = DIRECTION('',(0.,-0.500000000000002,-0.866025403784438)) ;
#2758 = DIRECTION('',(0.,0.499999999999999,-0.866025403784439)) ;
#2759 = DIRECTION('center_axis',(1.,0.,0.)) ;
#2760 = DIRECTION('ref_axis',(0.,0.,-1.)) ;
#2761 = DIRECTION('',(0.,0.499999999999999,-0.866025403784439)) ;
#2762 = DIRECTION('',(0.,1.,2.3112532288264E-16)) ;
#2763 = DIRECTION('center_axis',(1.,0.,0.)) ;
#2764 = DIRECTION('ref_axis',(0.,0.,-1.)) ;
#2765 = DIRECTION('center_axis',(1.,0.,0.)) ;
#2766 = DIRECTION('ref_axis',(0.,0.,-1.)) ;
#2767 = DIRECTION('center_axis',(1.,0.,0.)) ;
#2768 = DIRECTION('ref_axis',(0.,0.,-1.)) ;
#2769 = DIRECTION('center_axis',(1.,0.,0.)) ;
#2770 = DIRECTION('ref_axis',(0.,0.,-1.)) ;
#2771 = DIRECTION('center_axis',(1.,0.,0.)) ;
#2772 = DIRECTION('ref_axis',(0.,0.,-1.)) ;
#2773 = DIRECTION('center_axis',(-1.,0.,0.)) ;
#2774 = DIRECTION('ref_axis',(0.,0.,1.)) ;
#2775 = DIRECTION('center_axis',(1.,0.,0.)) ;
#2776 = DIRECTION('ref_axis',(0.,0.,-1.)) ;
#2777 = DIRECTION('center_axis',(1.,0.,0.)) ;
#2778 = DIRECTION('ref_axis',(0.,0.,-1.)) ;
#2779 = DIRECTION('center_axis',(1.,0.,0.)) ;
#2780 = DIRECTION('ref_axis',(0.,0.,-1.)) ;
#2781 = DIRECTION('center_axis',(1.,0.,0.)) ;
#2782 = DIRECTION('ref_axis',(0.,0.,-1.)) ;
#2783 = DIRECTION('center_axis',(1.,0.,0.)) ;
#2784 = DIRECTION('ref_axis',(0.,0.,-1.)) ;
#2785 = DIRECTION('center_axis',(1.,0.,0.)) ;
#2786 = DIRECTION('ref_axis',(0.,0.,-1.)) ;
#2787 = DIRECTION('center_axis',(1.,0.,0.)) ;
#2788 = DIRECTION('ref_axis',(0.,0.,-1.)) ;
#2789 = DIRECTION('center_axis',(0.,-2.3112532288264E-16,1.)) ;
#2790 = DIRECTION('ref_axis',(0.,-1.,-2.3112532288264E-16)) ;
#2791 = DIRECTION('',(-1.,0.,0.)) ;
#2792 = DIRECTION('',(-1.,0.,0.)) ;
#2793 = DIRECTION('center_axis',(0.,0.866025403784439,0.499999999999999)) ;
#2794 = DIRECTION('ref_axis',(0.,-0.499999999999999,0.866025403784439)) ;
#2795 = DIRECTION('',(-1.,0.,0.)) ;
#2796 = DIRECTION('center_axis',(0.,0.866025403784438,-0.500000000000002)) ;
#2797 = DIRECTION('ref_axis',(0.,0.500000000000002,0.866025403784438)) ;
#2798 = DIRECTION('',(-1.,0.,0.)) ;
#2799 = DIRECTION('center_axis',(0.,-2.3112532288264E-16,-1.)) ;
#2800 = DIRECTION('ref_axis',(0.,1.,-2.3112532288264E-16)) ;
#2801 = DIRECTION('',(-1.,0.,0.)) ;
#2802 = DIRECTION('center_axis',(0.,-0.866025403784438,-0.5)) ;
#2803 = DIRECTION('ref_axis',(0.,0.5,-0.866025403784438)) ;
#2804 = DIRECTION('',(-1.,0.,0.)) ;
#2805 = DIRECTION('center_axis',(0.,-0.866025403784438,0.500000000000002)) ;
#2806 = DIRECTION('ref_axis',(0.,-0.500000000000002,-0.866025403784438)) ;
#2807 = DIRECTION('',(0.293809879467176,-1.43347189327208E-17,-0.955863878764902)) ;
#2808 = DIRECTION('',(4.87890977618479E-17,1.,-1.5301084456074E-34)) ;
#2809 = DIRECTION('',(1.,3.61158816461081E-15,-6.88441343694035E-15)) ;
#2810 = DIRECTION('',(-6.88441343694036E-15,3.61158816461078E-15,-1.)) ;
#2811 = DIRECTION('',(1.,0.,0.)) ;
#2812 = DIRECTION('',(0.,0.,-1.)) ;
#2813 = DIRECTION('',(1.,0.,2.44929359829471E-16)) ;
#2814 = DIRECTION('',(2.44929359829471E-16,0.,-1.)) ;
#2815 = DIRECTION('',(0.,0.,1.)) ;
#2816 = DIRECTION('',(1.,0.,0.)) ;
#2817 = DIRECTION('',(0.,0.,1.)) ;
#2818 = DIRECTION('',(1.,0.,0.)) ;
#2819 = DIRECTION('',(0.,0.,1.)) ;
#2820 = DIRECTION('',(1.,0.,0.)) ;
#2821 = DIRECTION('',(0.,0.,1.)) ;
#2822 = DIRECTION('',(1.,0.,0.)) ;
#2823 = CARTESIAN_POINT('',(0.,0.,0.)) ;
#2824 = CARTESIAN_POINT('',(0.,0.,0.)) ;
#2825 = CARTESIAN_POINT('',(0.,0.,0.)) ;
#2826 = CARTESIAN_POINT('Origin',(-200.,-45.,-10.)) ;
#2827 = CARTESIAN_POINT('',(-200.,45.,0.)) ;
#2828 = CARTESIAN_POINT('',(-200.,-45.,0.)) ;
#2829 = CARTESIAN_POINT('',(-200.,-45.,0.)) ;
#2830 = CARTESIAN_POINT('',(-200.,45.,-10.)) ;
#2831 = CARTESIAN_POINT('',(-200.,45.,-10.)) ;
#2832 = CARTESIAN_POINT('',(-200.,-45.,-10.)) ;
#2833 = CARTESIAN_POINT('',(-200.,-45.,-10.)) ;
#2834 = CARTESIAN_POINT('',(-200.,-45.,-10.)) ;
#2835 = CARTESIAN_POINT('Origin',(200.,45.,-10.)) ;
#2836 = CARTESIAN_POINT('',(200.,45.,0.)) ;
#2837 = CARTESIAN_POINT('',(200.,45.,0.)) ;
#2838 = CARTESIAN_POINT('',(200.,45.,-10.)) ;
#2839 = CARTESIAN_POINT('',(200.,45.,-10.)) ;
#2840 = CARTESIAN_POINT('',(200.,45.,-10.)) ;
#2841 = CARTESIAN_POINT('Origin',(200.,-45.,-10.)) ;
#2842 = CARTESIAN_POINT('',(200.,-45.,0.)) ;
#2843 = CARTESIAN_POINT('',(200.,-45.,0.)) ;
#2844 = CARTESIAN_POINT('',(200.,-45.,-10.)) ;
#2845 = CARTESIAN_POINT('',(200.,-45.,-10.)) ;
#2846 = CARTESIAN_POINT('',(200.,-45.,-10.)) ;
#2847 = CARTESIAN_POINT('Origin',(200.,-45.,-10.)) ;
#2848 = CARTESIAN_POINT('',(200.,-45.,0.)) ;
#2849 = CARTESIAN_POINT('',(200.,-45.,-10.)) ;
#2850 = CARTESIAN_POINT('Origin',(0.,0.,-10.)) ;
#2851 = CARTESIAN_POINT('Origin',(0.,0.,0.)) ;
#2852 = CARTESIAN_POINT('',(0.,0.,0.)) ;
#2853 = CARTESIAN_POINT('Origin',(-1.38777878078145E-14,3.46944695195361E-15,
0.)) ;
#2854 = CARTESIAN_POINT('',(20.,1.02015335365891E-15,0.)) ;
#2855 = CARTESIAN_POINT('Origin',(-1.38777878078145E-14,3.46944695195361E-15,
0.)) ;
#2856 = CARTESIAN_POINT('',(20.,1.02015335365891E-15,-10.)) ;
#2857 = CARTESIAN_POINT('',(20.,1.0201533536589E-15,0.)) ;
#2858 = CARTESIAN_POINT('Origin',(-1.38777878078145E-14,3.46944695195361E-15,
-10.)) ;
#2859 = CARTESIAN_POINT('Origin',(-120.,-25.,-10.)) ;
#2860 = CARTESIAN_POINT('',(-120.,25.,0.)) ;
#2861 = CARTESIAN_POINT('',(-120.,-25.,0.)) ;
#2862 = CARTESIAN_POINT('',(-120.,-25.,0.)) ;
#2863 = CARTESIAN_POINT('',(-120.,25.,-10.)) ;
#2864 = CARTESIAN_POINT('',(-120.,25.,-10.)) ;
#2865 = CARTESIAN_POINT('',(-120.,-25.,-10.)) ;
#2866 = CARTESIAN_POINT('',(-120.,-25.,-10.)) ;
#2867 = CARTESIAN_POINT('',(-120.,-25.,-10.)) ;
#2868 = CARTESIAN_POINT('Origin',(120.,25.,-10.)) ;
#2869 = CARTESIAN_POINT('',(120.,25.,0.)) ;
#2870 = CARTESIAN_POINT('',(120.,25.,0.)) ;
#2871 = CARTESIAN_POINT('',(120.,25.,-10.)) ;
#2872 = CARTESIAN_POINT('',(120.,25.,-10.)) ;
#2873 = CARTESIAN_POINT('',(120.,25.,-10.)) ;
#2874 = CARTESIAN_POINT('Origin',(120.,-25.,-10.)) ;
#2875 = CARTESIAN_POINT('',(120.,-25.,0.)) ;
#2876 = CARTESIAN_POINT('',(120.,-25.,0.)) ;
#2877 = CARTESIAN_POINT('',(120.,-25.,-10.)) ;
#2878 = CARTESIAN_POINT('',(120.,-25.,-10.)) ;
#2879 = CARTESIAN_POINT('',(120.,-25.,-10.)) ;
#2880 = CARTESIAN_POINT('Origin',(120.,-25.,-10.)) ;
#2881 = CARTESIAN_POINT('',(120.,-25.,0.)) ;
#2882 = CARTESIAN_POINT('',(120.,-25.,-10.)) ;
#2883 = CARTESIAN_POINT('Origin',(0.,0.,-10.)) ;
#2884 = CARTESIAN_POINT('Origin',(0.,0.,0.)) ;
#2885 = CARTESIAN_POINT('',(0.,0.,0.)) ;
#2886 = CARTESIAN_POINT('Origin',(-300.,79.9999999999999,-22.)) ;
#2887 = CARTESIAN_POINT('',(-315.,79.9999999999999,-20.)) ;
#2888 = CARTESIAN_POINT('Origin',(-300.,79.9999999999999,-20.)) ;
#2889 = CARTESIAN_POINT('',(-315.,79.9999999999999,0.)) ;
#2890 = CARTESIAN_POINT('',(-315.,79.9999999999999,-22.)) ;
#2891 = CARTESIAN_POINT('Origin',(-300.,79.9999999999999,0.)) ;
#2892 = CARTESIAN_POINT('Origin',(-100.,79.9999999999999,-22.)) ;
#2893 = CARTESIAN_POINT('',(-115.,79.9999999999999,-20.)) ;
#2894 = CARTESIAN_POINT('Origin',(-100.,79.9999999999999,-20.)) ;
#2895 = CARTESIAN_POINT('',(-115.,79.9999999999999,0.)) ;
#2896 = CARTESIAN_POINT('',(-115.,79.9999999999999,-22.)) ;
#2897 = CARTESIAN_POINT('Origin',(-100.,79.9999999999999,0.)) ;
#2898 = CARTESIAN_POINT('Origin',(-80.,300.,-20.)) ;
#2899 = CARTESIAN_POINT('',(-165.,300.,0.)) ;
#2900 = CARTESIAN_POINT('',(-165.,300.,-20.)) ;
#2901 = CARTESIAN_POINT('',(-165.,300.,-20.)) ;
#2902 = CARTESIAN_POINT('',(-80.,300.,0.)) ;
#2903 = CARTESIAN_POINT('',(-80.,300.,0.)) ;
#2904 = CARTESIAN_POINT('',(-80.,300.,-20.)) ;
#2905 = CARTESIAN_POINT('',(-80.,300.,-20.)) ;
#2906 = CARTESIAN_POINT('',(-80.,300.,-20.)) ;
#2907 = CARTESIAN_POINT('Origin',(0.,0.,-20.)) ;
#2908 = CARTESIAN_POINT('',(0.,0.,0.)) ;
#2909 = CARTESIAN_POINT('',(0.,150.,0.)) ;
#2910 = CARTESIAN_POINT('',(0.,0.,0.)) ;
#2911 = CARTESIAN_POINT('',(0.,0.,-20.)) ;
#2912 = CARTESIAN_POINT('',(0.,0.,-20.)) ;
#2913 = CARTESIAN_POINT('',(0.,150.,-20.)) ;
#2914 = CARTESIAN_POINT('',(0.,0.,-20.)) ;
#2915 = CARTESIAN_POINT('',(0.,150.,-20.)) ;
#2916 = CARTESIAN_POINT('Origin',(0.,0.,-20.)) ;
#2917 = CARTESIAN_POINT('',(-400.,0.,0.)) ;
#2918 = CARTESIAN_POINT('',(0.,0.,0.)) ;
#2919 = CARTESIAN_POINT('',(-400.,0.,-20.)) ;
#2920 = CARTESIAN_POINT('',(-400.,0.,-20.)) ;
#2921 = CARTESIAN_POINT('',(0.,0.,-20.)) ;
#2922 = CARTESIAN_POINT('Origin',(-400.,0.,-20.)) ;
#2923 = CARTESIAN_POINT('',(-400.,150.,0.)) ;
#2924 = CARTESIAN_POINT('',(-400.,0.,0.)) ;
#2925 = CARTESIAN_POINT('',(-400.,150.,-20.)) ;
#2926 = CARTESIAN_POINT('',(-400.,150.,-20.)) ;
#2927 = CARTESIAN_POINT('',(-400.,0.,-20.)) ;
#2928 = CARTESIAN_POINT('Origin',(-400.,150.,-20.)) ;
#2929 = CARTESIAN_POINT('',(-320.,300.,0.)) ;
#2930 = CARTESIAN_POINT('',(-400.,150.,0.)) ;
#2931 = CARTESIAN_POINT('',(-320.,300.,-20.)) ;
#2932 = CARTESIAN_POINT('',(-320.,300.,-20.)) ;
#2933 = CARTESIAN_POINT('',(-400.,150.,-20.)) ;
#2934 = CARTESIAN_POINT('Origin',(-80.,300.,-20.)) ;
#2935 = CARTESIAN_POINT('',(-235.,300.,-20.)) ;
#2936 = CARTESIAN_POINT('',(-235.,300.,0.)) ;
#2937 = CARTESIAN_POINT('',(-235.,300.,-20.)) ;
#2938 = CARTESIAN_POINT('',(-80.,300.,-20.)) ;
#2939 = CARTESIAN_POINT('',(-80.,300.,0.)) ;
#2940 = CARTESIAN_POINT('Origin',(0.,150.,-20.)) ;
#2941 = CARTESIAN_POINT('',(0.,150.,0.)) ;
#2942 = CARTESIAN_POINT('',(0.,150.,-20.)) ;
#2943 = CARTESIAN_POINT('Origin',(0.,0.,-20.)) ;
#2944 = CARTESIAN_POINT('',(-235.,150.,-20.)) ;
#2945 = CARTESIAN_POINT('',(-165.,150.,-20.)) ;
#2946 = CARTESIAN_POINT('',(0.,150.,-20.)) ;
#2947 = CARTESIAN_POINT('',(-165.,0.,-20.)) ;
#2948 = CARTESIAN_POINT('',(-235.,-2.1741867565576E-14,-20.)) ;
#2949 = CARTESIAN_POINT('Origin',(0.,0.,0.)) ;
#2950 = CARTESIAN_POINT('',(-165.,150.,0.)) ;
#2951 = CARTESIAN_POINT('',(-165.,450.,0.)) ;
#2952 = CARTESIAN_POINT('',(-235.,150.,0.)) ;
#2953 = CARTESIAN_POINT('',(-235.,150.,0.)) ;
#2954 = CARTESIAN_POINT('',(-235.,-2.1741867565576E-14,0.)) ;
#2955 = CARTESIAN_POINT('Origin',(-235.,150.,-22.)) ;
#2956 = CARTESIAN_POINT('',(-235.,150.,-22.)) ;
#2957 = CARTESIAN_POINT('',(-165.,150.,-22.)) ;
#2958 = CARTESIAN_POINT('Origin',(-165.,450.,-22.)) ;
#2959 = CARTESIAN_POINT('Origin',(-235.,450.,-22.)) ;
#2960 = CARTESIAN_POINT('',(0.,0.,0.)) ;
#2961 = CARTESIAN_POINT('',(-200.000000000001,-9.99999999999837,-44.9999999999974)) ;
#2962 = CARTESIAN_POINT('',(-200.,290.000000000004,-44.999999999997)) ;
#2963 = CARTESIAN_POINT('',(0.,0.,-70.)) ;
#2964 = CARTESIAN_POINT('',(0.,0.,0.)) ;
#2965 = CARTESIAN_POINT('',(0.,0.,0.)) ;
#2966 = CARTESIAN_POINT('Origin',(150.,-25.,0.)) ;
#2967 = CARTESIAN_POINT('',(155.,-22.7551020408163,2.78562319867339E-15)) ;
#2968 = CARTESIAN_POINT('',(145.,-22.7551020408163,-1.70559836960368E-15)) ;
#2969 = CARTESIAN_POINT('Ctrl Pts',(155.,-22.7551020408163,2.77555756156289E-16)) ;
#2970 = CARTESIAN_POINT('Ctrl Pts',(155.,-22.7551020408163,0.630003217984992)) ;
#2971 = CARTESIAN_POINT('Ctrl Pts',(154.873673921497,-22.7263022754814,1.30061158958556)) ;
#2972 = CARTESIAN_POINT('Ctrl Pts',(154.36275982174,-22.6222410731759,2.53191912872512)) ;
#2973 = CARTESIAN_POINT('Ctrl Pts',(153.978283678305,-22.5483975458322,3.09278413356067)) ;
#2974 = CARTESIAN_POINT('Ctrl Pts',(153.092747694998,-22.4091175126403,3.97832011686759)) ;
#2975 = CARTESIAN_POINT('Ctrl Pts',(152.53189805439,-22.3344796638631,4.36276776282476)) ;
#2976 = CARTESIAN_POINT('Ctrl Pts',(151.30064431178,-22.228588638716,4.87366114728546)) ;
#2977 = CARTESIAN_POINT('Ctrl Pts',(150.630055067615,-22.19897900553,5.00000000000002)) ;
#2978 = CARTESIAN_POINT('Ctrl Pts',(150.,-22.19897900553,5.00000000000002)) ;
#2979 = CARTESIAN_POINT('Ctrl Pts',(149.369944932385,-22.19897900553,5.00000000000002)) ;
#2980 = CARTESIAN_POINT('Ctrl Pts',(148.69935568822,-22.228588638716,4.87366114728546)) ;
#2981 = CARTESIAN_POINT('Ctrl Pts',(147.46810194561,-22.3344796638631,4.36276776282476)) ;
#2982 = CARTESIAN_POINT('Ctrl Pts',(146.907252305002,-22.4091175126403,3.97832011686759)) ;
#2983 = CARTESIAN_POINT('Ctrl Pts',(146.021716321695,-22.5483975458322,3.09278413356067)) ;
#2984 = CARTESIAN_POINT('Ctrl Pts',(145.63724017826,-22.6222410731759,2.53191912872511)) ;
#2985 = CARTESIAN_POINT('Ctrl Pts',(145.126326078503,-22.7263022754814,1.30061158958555)) ;
#2986 = CARTESIAN_POINT('Ctrl Pts',(145.,-22.7551020408163,0.630003217984992)) ;
#2987 = CARTESIAN_POINT('Ctrl Pts',(145.,-22.7551020408163,-9.0205620750794E-16)) ;
#2988 = CARTESIAN_POINT('',(150.,-22.19897900553,-5.00000000000002)) ;
#2989 = CARTESIAN_POINT('Ctrl Pts',(145.,-22.7551020408163,-9.71445146547012E-16)) ;
#2990 = CARTESIAN_POINT('Ctrl Pts',(145.,-22.7551020408163,-0.630003217984994)) ;
#2991 = CARTESIAN_POINT('Ctrl Pts',(145.126326078503,-22.7263022754814,-1.30061158958556)) ;
#2992 = CARTESIAN_POINT('Ctrl Pts',(145.63724017826,-22.6222410731759,-2.53191912872513)) ;
#2993 = CARTESIAN_POINT('Ctrl Pts',(146.021716321695,-22.5483975458322,-3.09278413356067)) ;
#2994 = CARTESIAN_POINT('Ctrl Pts',(146.907252305002,-22.4091175126403,-3.97832011686759)) ;
#2995 = CARTESIAN_POINT('Ctrl Pts',(147.46810194561,-22.3344796638631,-4.36276776282476)) ;
#2996 = CARTESIAN_POINT('Ctrl Pts',(148.69935568822,-22.228588638716,-4.87366114728546)) ;
#2997 = CARTESIAN_POINT('Ctrl Pts',(149.369944932385,-22.19897900553,-5.00000000000002)) ;
#2998 = CARTESIAN_POINT('Ctrl Pts',(150.,-22.19897900553,-5.00000000000002)) ;
#2999 = CARTESIAN_POINT('',(150.,22.19897900553,-5.00000000000002)) ;
#3000 = CARTESIAN_POINT('',(150.,-25.,-5.00000000000002)) ;
#3001 = CARTESIAN_POINT('Ctrl Pts',(150.,22.19897900553,5.00000000000002)) ;
#3002 = CARTESIAN_POINT('Ctrl Pts',(150.630055067615,22.19897900553,5.00000000000002)) ;
#3003 = CARTESIAN_POINT('Ctrl Pts',(151.30064431178,22.228588638716,4.87366114728546)) ;
#3004 = CARTESIAN_POINT('Ctrl Pts',(152.53189805439,22.3344796638632,4.36276776282476)) ;
#3005 = CARTESIAN_POINT('Ctrl Pts',(153.092747694998,22.4091175126403,3.97832011686759)) ;
#3006 = CARTESIAN_POINT('Ctrl Pts',(153.978283678305,22.5483975458322,3.09278413356067)) ;
#3007 = CARTESIAN_POINT('Ctrl Pts',(154.36275982174,22.6222410731759,2.53191912872511)) ;
#3008 = CARTESIAN_POINT('Ctrl Pts',(154.873673921497,22.7263022754814,1.30061158958554)) ;
#3009 = CARTESIAN_POINT('Ctrl Pts',(155.,22.7551020408163,0.630003217984991)) ;
#3010 = CARTESIAN_POINT('Ctrl Pts',(155.,22.7551020408163,-0.630003217984991)) ;
#3011 = CARTESIAN_POINT('Ctrl Pts',(154.873673921497,22.7263022754814,-1.30061158958554)) ;
#3012 = CARTESIAN_POINT('Ctrl Pts',(154.36275982174,22.6222410731759,-2.5319191287251)) ;
#3013 = CARTESIAN_POINT('Ctrl Pts',(153.978283678305,22.5483975458322,-3.09278413356067)) ;
#3014 = CARTESIAN_POINT('Ctrl Pts',(153.092747694998,22.4091175126403,-3.97832011686758)) ;
#3015 = CARTESIAN_POINT('Ctrl Pts',(152.53189805439,22.3344796638632,-4.36276776282476)) ;
#3016 = CARTESIAN_POINT('Ctrl Pts',(151.30064431178,22.228588638716,-4.87366114728546)) ;
#3017 = CARTESIAN_POINT('Ctrl Pts',(150.630055067615,22.19897900553,-5.00000000000002)) ;
#3018 = CARTESIAN_POINT('Ctrl Pts',(149.369944932385,22.19897900553,-5.00000000000002)) ;
#3019 = CARTESIAN_POINT('Ctrl Pts',(148.69935568822,22.228588638716,-4.87366114728546)) ;
#3020 = CARTESIAN_POINT('Ctrl Pts',(147.46810194561,22.3344796638631,-4.36276776282476)) ;
#3021 = CARTESIAN_POINT('Ctrl Pts',(146.907252305002,22.4091175126403,-3.97832011686759)) ;
#3022 = CARTESIAN_POINT('Ctrl Pts',(146.021716321695,22.5483975458322,-3.09278413356067)) ;
#3023 = CARTESIAN_POINT('Ctrl Pts',(145.63724017826,22.6222410731759,-2.53191912872511)) ;
#3024 = CARTESIAN_POINT('Ctrl Pts',(145.126326078503,22.7263022754814,-1.30061158958555)) ;
#3025 = CARTESIAN_POINT('Ctrl Pts',(145.,22.7551020408163,-0.630003217984993)) ;
#3026 = CARTESIAN_POINT('Ctrl Pts',(145.,22.7551020408163,0.630003217984992)) ;
#3027 = CARTESIAN_POINT('Ctrl Pts',(145.126326078503,22.7263022754814,1.30061158958556)) ;
#3028 = CARTESIAN_POINT('Ctrl Pts',(145.63724017826,22.6222410731759,2.53191912872512)) ;
#3029 = CARTESIAN_POINT('Ctrl Pts',(146.021716321695,22.5483975458322,3.09278413356067)) ;
#3030 = CARTESIAN_POINT('Ctrl Pts',(146.907252305002,22.4091175126403,3.97832011686759)) ;
#3031 = CARTESIAN_POINT('Ctrl Pts',(147.46810194561,22.3344796638632,4.36276776282476)) ;
#3032 = CARTESIAN_POINT('Ctrl Pts',(148.69935568822,22.228588638716,4.87366114728546)) ;
#3033 = CARTESIAN_POINT('Ctrl Pts',(149.369944932385,22.19897900553,5.00000000000002)) ;
#3034 = CARTESIAN_POINT('Ctrl Pts',(150.,22.19897900553,5.00000000000002)) ;
#3035 = CARTESIAN_POINT('Ctrl Pts',(150.,-22.19897900553,-5.00000000000002)) ;
#3036 = CARTESIAN_POINT('Ctrl Pts',(150.630055067615,-22.19897900553,-5.00000000000002)) ;
#3037 = CARTESIAN_POINT('Ctrl Pts',(151.30064431178,-22.228588638716,-4.87366114728547)) ;
#3038 = CARTESIAN_POINT('Ctrl Pts',(152.53189805439,-22.3344796638631,-4.36276776282477)) ;
#3039 = CARTESIAN_POINT('Ctrl Pts',(153.092747694998,-22.4091175126403,-3.97832011686758)) ;
#3040 = CARTESIAN_POINT('Ctrl Pts',(153.978283678305,-22.5483975458322,-3.09278413356067)) ;
#3041 = CARTESIAN_POINT('Ctrl Pts',(154.36275982174,-22.6222410731759,-2.53191912872511)) ;
#3042 = CARTESIAN_POINT('Ctrl Pts',(154.873673921497,-22.7263022754814,-1.30061158958555)) ;
#3043 = CARTESIAN_POINT('Ctrl Pts',(155.,-22.7551020408163,-0.630003217984992)) ;
#3044 = CARTESIAN_POINT('Ctrl Pts',(155.,-22.7551020408163,0.)) ;
#3045 = CARTESIAN_POINT('Origin',(20.0000000000002,5.69529073405534E-16,0.)) ;
#3046 = CARTESIAN_POINT('',(20.0000000000002,-22.7551020408163,-2.78669628785571E-15)) ;
#3047 = CARTESIAN_POINT('Origin',(20.0000000000002,5.69529073405534E-16,0.)) ;
#3048 = CARTESIAN_POINT('',(12.2448979591838,-15.,-1.83697019872103E-15)) ;
#3049 = CARTESIAN_POINT('',(20.0000000000002,-22.7551020408163,-2.78669628785571E-15)) ;
#3050 = CARTESIAN_POINT('Origin',(12.2448979591838,3.48691269431959E-16,0.)) ;
#3051 = CARTESIAN_POINT('Origin',(160.,4.55623258724423E-15,0.)) ;
#3052 = CARTESIAN_POINT('',(160.,-22.7551020408163,-2.78669628785571E-15)) ;
#3053 = CARTESIAN_POINT('Origin',(160.,4.55623258724423E-15,0.)) ;
#3054 = CARTESIAN_POINT('',(160.,-22.7551020408163,-2.78669628785571E-15)) ;
#3055 = CARTESIAN_POINT('',(160.,-22.7551020408163,-2.78669628785571E-15)) ;
#3056 = CARTESIAN_POINT('Origin',(160.,4.55623258724423E-15,0.)) ;
#3057 = CARTESIAN_POINT('',(0.,-15.,-1.83697019872103E-15)) ;
#3058 = CARTESIAN_POINT('',(160.,-15.,-1.83697019872103E-15)) ;
#3059 = CARTESIAN_POINT('Origin',(0.,0.,0.)) ;
#3060 = CARTESIAN_POINT('Origin',(2.13573402527073E-16,6.08181310226549E-33,
0.)) ;
#3061 = CARTESIAN_POINT('Origin',(160.,22.7551020408163,0.)) ;
#3062 = CARTESIAN_POINT('',(0.,0.,0.)) ;
#3063 = CARTESIAN_POINT('Origin',(0.,0.,150.)) ;
#3064 = CARTESIAN_POINT('',(5.,-6.12323399573677E-16,0.)) ;
#3065 = CARTESIAN_POINT('Origin',(0.,0.,0.)) ;
#3066 = CARTESIAN_POINT('',(5.,-6.12323399573677E-16,150.)) ;
#3067 = CARTESIAN_POINT('',(5.,-6.12323399573677E-16,150.)) ;
#3068 = CARTESIAN_POINT('Origin',(0.,0.,150.)) ;
#3069 = CARTESIAN_POINT('Origin',(0.,0.,150.)) ;
#3070 = CARTESIAN_POINT('Origin',(0.,0.,0.)) ;
#3071 = CARTESIAN_POINT('',(0.,0.,0.)) ;
#3072 = CARTESIAN_POINT('Origin',(-25.,0.,0.)) ;
#3073 = CARTESIAN_POINT('',(-25.,-1.83697019872103E-15,15.)) ;
#3074 = CARTESIAN_POINT('Origin',(-25.,0.,0.)) ;
#3075 = CARTESIAN_POINT('',(25.,-1.83697019872103E-15,15.)) ;
#3076 = CARTESIAN_POINT('',(-25.,-1.83697019872103E-15,15.)) ;
#3077 = CARTESIAN_POINT('Origin',(25.,0.,0.)) ;
#3078 = CARTESIAN_POINT('Origin',(0.,16.254058593968,0.)) ;
#3079 = CARTESIAN_POINT('',(-1.83697019872103E-15,16.254058593968,-15.)) ;
#3080 = CARTESIAN_POINT('Origin',(0.,16.254058593968,0.)) ;
#3081 = CARTESIAN_POINT('',(-1.83697019872103E-15,25.254058593968,-15.)) ;
#3082 = CARTESIAN_POINT('',(-1.83697019872103E-15,16.254058593968,-15.)) ;
#3083 = CARTESIAN_POINT('Origin',(0.,25.254058593968,0.)) ;
#3084 = CARTESIAN_POINT('Origin',(-25.,-25.254058593968,50.)) ;
#3085 = CARTESIAN_POINT('',(-25.,25.254058593968,-50.)) ;
#3086 = CARTESIAN_POINT('',(-25.,-25.254058593968,-50.)) ;
#3087 = CARTESIAN_POINT('',(-25.,-25.254058593968,-50.)) ;
#3088 = CARTESIAN_POINT('',(-25.,-25.254058593968,50.)) ;
#3089 = CARTESIAN_POINT('',(-25.,-25.254058593968,50.)) ;
#3090 = CARTESIAN_POINT('',(-25.,25.254058593968,50.)) ;
#3091 = CARTESIAN_POINT('',(-25.,-25.254058593968,50.)) ;
#3092 = CARTESIAN_POINT('',(-25.,25.254058593968,50.)) ;
#3093 = CARTESIAN_POINT('Origin',(25.,-25.254058593968,50.)) ;
#3094 = CARTESIAN_POINT('',(25.,-25.254058593968,-50.)) ;
#3095 = CARTESIAN_POINT('',(25.,-25.254058593968,-50.)) ;
#3096 = CARTESIAN_POINT('',(25.,-25.254058593968,50.)) ;
#3097 = CARTESIAN_POINT('',(25.,-25.254058593968,50.)) ;
#3098 = CARTESIAN_POINT('',(25.,-25.254058593968,50.)) ;
#3099 = CARTESIAN_POINT('Origin',(25.,-25.254058593968,50.)) ;
#3100 = CARTESIAN_POINT('',(25.,25.254058593968,-50.)) ;
#3101 = CARTESIAN_POINT('',(25.,-25.254058593968,-50.)) ;
#3102 = CARTESIAN_POINT('',(25.,25.254058593968,50.)) ;
#3103 = CARTESIAN_POINT('',(25.,25.254058593968,50.)) ;
#3104 = CARTESIAN_POINT('',(25.,-25.254058593968,50.)) ;
#3105 = CARTESIAN_POINT('Origin',(25.,25.254058593968,50.)) ;
#3106 = CARTESIAN_POINT('',(25.,25.254058593968,-50.)) ;
#3107 = CARTESIAN_POINT('',(25.,25.254058593968,50.)) ;
#3108 = CARTESIAN_POINT('Origin',(0.,0.,50.)) ;
#3109 = CARTESIAN_POINT('Origin',(0.,0.,-50.)) ;
#3110 = CARTESIAN_POINT('Origin',(0.,16.254058593968,0.)) ;
#3111 = CARTESIAN_POINT('',(0.,0.,0.)) ;
#3112 = CARTESIAN_POINT('Origin',(127.,0.,0.)) ;
#3113 = CARTESIAN_POINT('',(87.,-4.16379911710099E-16,3.39999999999999)) ;
#3114 = CARTESIAN_POINT('Origin',(87.,0.,0.)) ;
#3115 = CARTESIAN_POINT('',(127.,-4.16379911710099E-16,3.39999999999999)) ;
#3116 = CARTESIAN_POINT('',(127.,-4.16379911710099E-16,3.39999999999999)) ;
#3117 = CARTESIAN_POINT('Origin',(127.,0.,0.)) ;
#3118 = CARTESIAN_POINT('Origin',(87.,0.,0.)) ;
#3119 = CARTESIAN_POINT('',(84.9570738953063,-1.18034773709391E-14,0.)) ;
#3120 = CARTESIAN_POINT('',(87.,-4.16379911710099E-16,3.39999999999999)) ;
#3121 = CARTESIAN_POINT('Origin',(127.,0.,0.)) ;
#3122 = CARTESIAN_POINT('',(127.,-1.53080849893419E-15,12.5)) ;
#3123 = CARTESIAN_POINT('Origin',(127.,0.,0.)) ;
#3124 = CARTESIAN_POINT('',(77.,-1.53080849893419E-15,12.5)) ;
#3125 = CARTESIAN_POINT('',(127.,-1.53080849893419E-15,12.5)) ;
#3126 = CARTESIAN_POINT('Origin',(77.,0.,0.)) ;
#3127 = CARTESIAN_POINT('Origin',(127.,0.,0.)) ;
#3128 = CARTESIAN_POINT('',(77.,-1.83697019872103E-15,15.)) ;
#3129 = CARTESIAN_POINT('Origin',(77.,0.,0.)) ;
#3130 = CARTESIAN_POINT('',(5.00000000000002,-1.83697019872103E-15,15.)) ;
#3131 = CARTESIAN_POINT('',(127.,-1.83697019872103E-15,15.)) ;
#3132 = CARTESIAN_POINT('Origin',(5.,0.,0.)) ;
#3133 = CARTESIAN_POINT('Origin',(127.,0.,0.)) ;
#3134 = CARTESIAN_POINT('',(5.,-2.14313189850787E-15,17.5)) ;
#3135 = CARTESIAN_POINT('Origin',(5.,0.,0.)) ;
#3136 = CARTESIAN_POINT('',(0.,-2.14313189850787E-15,17.5)) ;
#3137 = CARTESIAN_POINT('',(127.,-2.14313189850787E-15,17.5)) ;
#3138 = CARTESIAN_POINT('Origin',(0.,0.,0.)) ;
#3139 = CARTESIAN_POINT('Origin',(0.,0.,0.)) ;
#3140 = CARTESIAN_POINT('Origin',(5.,17.5,0.)) ;
#3141 = CARTESIAN_POINT('Origin',(77.,15.,0.)) ;
#3142 = CARTESIAN_POINT('Origin',(127.,12.5,0.)) ;
#3143 = CARTESIAN_POINT('',(0.,0.,0.)) ;
#3144 = CARTESIAN_POINT('Origin',(147.,-1.73472347597681E-15,0.)) ;
#3145 = CARTESIAN_POINT('',(107.,-2.15110338768691E-15,3.39999999999999)) ;
#3146 = CARTESIAN_POINT('Origin',(107.,-1.73472347597681E-15,0.)) ;
#3147 = CARTESIAN_POINT('',(147.,-2.15110338768691E-15,3.39999999999999)) ;
#3148 = CARTESIAN_POINT('',(147.,-2.15110338768691E-15,3.39999999999999)) ;
#3149 = CARTESIAN_POINT('Origin',(147.,-1.73472347597681E-15,0.)) ;
#3150 = CARTESIAN_POINT('Origin',(107.,-1.73472347597681E-15,0.)) ;
#3151 = CARTESIAN_POINT('',(104.957073895306,-1.35382008469159E-14,0.)) ;
#3152 = CARTESIAN_POINT('',(107.,-2.15110338768691E-15,3.39999999999999)) ;
#3153 = CARTESIAN_POINT('Origin',(147.,-1.73472347597681E-15,0.)) ;
#3154 = CARTESIAN_POINT('',(147.,-12.5,-1.53080849893419E-15)) ;
#3155 = CARTESIAN_POINT('Origin',(147.,-1.73472347597681E-15,0.)) ;
#3156 = CARTESIAN_POINT('',(97.,-12.5,-1.53080849893419E-15)) ;
#3157 = CARTESIAN_POINT('',(147.,-12.5,-1.53080849893419E-15)) ;
#3158 = CARTESIAN_POINT('Origin',(97.,-1.14468147734524E-15,0.)) ;
#3159 = CARTESIAN_POINT('Origin',(147.,-1.73472347597681E-15,0.)) ;
#3160 = CARTESIAN_POINT('',(97.,-15.,-1.83697019872103E-15)) ;
#3161 = CARTESIAN_POINT('Origin',(97.,-1.14468147734524E-15,0.)) ;
#3162 = CARTESIAN_POINT('',(5.,-15.,-1.83697019872103E-15)) ;
#3163 = CARTESIAN_POINT('',(147.,-15.,-1.83697019872103E-15)) ;
#3164 = CARTESIAN_POINT('Origin',(5.,-5.90041998631564E-17,0.)) ;
#3165 = CARTESIAN_POINT('Origin',(147.,-1.73472347597681E-15,0.)) ;
#3166 = CARTESIAN_POINT('',(5.,-17.5,-2.14313189850787E-15)) ;
#3167 = CARTESIAN_POINT('Origin',(5.,-5.90041998631564E-17,0.)) ;
#3168 = CARTESIAN_POINT('',(0.,-17.5,-2.14313189850787E-15)) ;
#3169 = CARTESIAN_POINT('',(147.,-17.5,-2.14313189850787E-15)) ;
#3170 = CARTESIAN_POINT('Origin',(0.,3.85185988877447E-31,0.)) ;
#3171 = CARTESIAN_POINT('Origin',(-1.03257349760524E-16,1.21852346052197E-33,
0.)) ;
#3172 = CARTESIAN_POINT('Origin',(5.,17.5,0.)) ;
#3173 = CARTESIAN_POINT('Origin',(97.,15.,0.)) ;
#3174 = CARTESIAN_POINT('Origin',(147.,12.5,0.)) ;
#3175 = CARTESIAN_POINT('',(-200.,240.875903950236,-44.9999999999981)) ;
#3176 = CARTESIAN_POINT('',(-87.8115175700917,390.875903950236,-12.2268759659618)) ;
#3177 = CARTESIAN_POINT('',(-200.,233.691743315453,-44.9999999999909)) ;
#3178 = CARTESIAN_POINT('',(-200.,233.691743315449,-75.0000000000001)) ;
#3179 = CARTESIAN_POINT('',(-300.000000000001,79.9999999999999,-94.9999999999976)) ;
#3180 = CARTESIAN_POINT('',(-100.000000000001,80.0000000000001,-94.9999999999991)) ;
#3181 = CARTESIAN_POINT('',(0.,0.,0.)) ;
#3182 = CARTESIAN_POINT('',(0.,0.,0.)) ;
#3183 = CARTESIAN_POINT('Origin',(0.,0.,0.)) ;
#3184 = CARTESIAN_POINT('',(50.,-6.12323399573677E-15,20.)) ;
#3185 = CARTESIAN_POINT('',(-50.,-6.12323399573677E-15,20.)) ;
#3186 = CARTESIAN_POINT('Origin',(0.,0.,20.)) ;
#3187 = CARTESIAN_POINT('',(-50.,-6.12323399573677E-15,-20.)) ;
#3188 = CARTESIAN_POINT('Origin',(-50.,-6.12323399573677E-15,0.)) ;
#3189 = CARTESIAN_POINT('',(50.,-6.12323399573677E-15,-20.)) ;
#3190 = CARTESIAN_POINT('Origin',(0.,0.,-20.)) ;
#3191 = CARTESIAN_POINT('Origin',(0.,0.,-20.)) ;
#3192 = CARTESIAN_POINT('Origin',(0.,0.,20.)) ;
#3193 = CARTESIAN_POINT('Origin',(0.,0.,-25.)) ;
#3194 = CARTESIAN_POINT('',(-12.5,-1.53080849893419E-15,-25.)) ;
#3195 = CARTESIAN_POINT('Origin',(0.,0.,-25.)) ;
#3196 = CARTESIAN_POINT('',(-12.5,-1.53080849893419E-15,25.)) ;
#3197 = CARTESIAN_POINT('',(-12.5,-1.53080849893419E-15,-25.)) ;
#3198 = CARTESIAN_POINT('Origin',(0.,0.,25.)) ;
#3199 = CARTESIAN_POINT('Origin',(0.,0.,25.)) ;
#3200 = CARTESIAN_POINT('',(50.,-6.12323399573677E-15,-25.)) ;
#3201 = CARTESIAN_POINT('Origin',(0.,0.,-25.)) ;
#3202 = CARTESIAN_POINT('',(50.,-6.12323399573677E-15,25.)) ;
#3203 = CARTESIAN_POINT('Origin',(0.,0.,25.)) ;
#3204 = CARTESIAN_POINT('',(50.,-6.12323399573677E-15,25.)) ;
#3205 = CARTESIAN_POINT('',(50.,-6.12323399573677E-15,25.)) ;
#3206 = CARTESIAN_POINT('Origin',(0.,0.,25.)) ;
#3207 = CARTESIAN_POINT('Origin',(0.,0.,25.)) ;
#3208 = CARTESIAN_POINT('Origin',(0.,0.,-25.)) ;
#3209 = CARTESIAN_POINT('',(0.,0.,0.)) ;
#3210 = CARTESIAN_POINT('Origin',(5.,0.,0.)) ;
#3211 = CARTESIAN_POINT('',(5.,-5.51091059616309E-16,-4.5)) ;
#3212 = CARTESIAN_POINT('Origin',(5.,0.,0.)) ;
#3213 = CARTESIAN_POINT('',(0.,-5.51091059616309E-16,-4.5)) ;
#3214 = CARTESIAN_POINT('',(5.,-5.51091059616309E-16,-4.5)) ;
#3215 = CARTESIAN_POINT('Origin',(0.,0.,0.)) ;
#3216 = CARTESIAN_POINT('Origin',(5.,0.,0.)) ;
#3217 = CARTESIAN_POINT('',(0.,-3.06161699786838E-15,-25.)) ;
#3218 = CARTESIAN_POINT('Origin',(0.,0.,0.)) ;
#3219 = CARTESIAN_POINT('',(5.,-3.06161699786838E-15,-25.)) ;
#3220 = CARTESIAN_POINT('',(5.,-3.06161699786838E-15,-25.)) ;
#3221 = CARTESIAN_POINT('Origin',(5.,0.,0.)) ;
#3222 = CARTESIAN_POINT('Origin',(5.,0.,0.)) ;
#3223 = CARTESIAN_POINT('Origin',(0.,0.,0.)) ;
#3224 = CARTESIAN_POINT('',(-200.,233.691743315449,26.9999999999999)) ;
#3225 = CARTESIAN_POINT('',(-200.,233.691743315449,56.9999999999999)) ;
#3226 = CARTESIAN_POINT('',(-300.,79.9999999999999,27.)) ;
#3227 = CARTESIAN_POINT('',(-100.,79.9999999999999,27.000000000001)) ;
#3228 = CARTESIAN_POINT('',(-300.,79.9999999999999,52.)) ;
#3229 = CARTESIAN_POINT('',(-100.,79.9999999999999,56.9999999999987)) ;
#3230 = CARTESIAN_POINT('',(0.,0.,0.)) ;
#3231 = CARTESIAN_POINT('',(0.,0.,0.)) ;
#3232 = CARTESIAN_POINT('Origin',(-5.5,0.,0.)) ;
#3233 = CARTESIAN_POINT('',(-5.5,-3.36777869765522E-15,27.5)) ;
#3234 = CARTESIAN_POINT('Origin',(-5.5,0.,0.)) ;
#3235 = CARTESIAN_POINT('',(-6.5,-3.24531401774049E-15,26.5)) ;
#3236 = CARTESIAN_POINT('Origin',(-5.5,-3.24531401774049E-15,26.5)) ;
#3237 = CARTESIAN_POINT('Origin',(-6.5,0.,0.)) ;
#3238 = CARTESIAN_POINT('Origin',(-20.6375,0.,0.)) ;
#3239 = CARTESIAN_POINT('',(5.5,-3.36777869765522E-15,27.5)) ;
#3240 = CARTESIAN_POINT('Origin',(5.5,0.,0.)) ;
#3241 = CARTESIAN_POINT('',(-20.6375,-3.36777869765522E-15,27.5)) ;
#3242 = CARTESIAN_POINT('Origin',(5.5,0.,0.)) ;
#3243 = CARTESIAN_POINT('',(6.5,-3.24531401774049E-15,26.5)) ;
#3244 = CARTESIAN_POINT('Origin',(6.5,0.,0.)) ;
#3245 = CARTESIAN_POINT('Origin',(5.5,-3.24531401774049E-15,26.5)) ;
#3246 = CARTESIAN_POINT('Origin',(-20.6375,0.,0.)) ;
#3247 = CARTESIAN_POINT('',(-6.5,-2.90853614797497E-15,23.75)) ;
#3248 = CARTESIAN_POINT('Origin',(-6.5,0.,0.)) ;
#3249 = CARTESIAN_POINT('',(-2.79508497187473,-2.90853614797496E-15,23.75)) ;
#3250 = CARTESIAN_POINT('',(-20.6375,-2.90853614797496E-15,23.75)) ;
#3251 = CARTESIAN_POINT('',(-2.79508497187473,2.90853614797496E-15,-23.75)) ;
#3252 = CARTESIAN_POINT('Origin',(-2.79508497187473,0.,0.)) ;
#3253 = CARTESIAN_POINT('Origin',(-2.79508497187473,0.,0.)) ;
#3254 = CARTESIAN_POINT('Origin',(-20.6375,0.,0.)) ;
#3255 = CARTESIAN_POINT('',(2.79508497187473,2.90853614797496E-15,-23.75)) ;
#3256 = CARTESIAN_POINT('',(2.79508497187473,-2.90853614797496E-15,23.75)) ;
#3257 = CARTESIAN_POINT('Origin',(2.79508497187473,0.,0.)) ;
#3258 = CARTESIAN_POINT('Origin',(2.79508497187473,0.,0.)) ;
#3259 = CARTESIAN_POINT('',(6.5,-2.90853614797497E-15,23.75)) ;
#3260 = CARTESIAN_POINT('',(-20.6375,-2.90853614797496E-15,23.75)) ;
#3261 = CARTESIAN_POINT('Origin',(6.5,0.,0.)) ;
#3262 = CARTESIAN_POINT('Origin',(0.,0.,0.)) ;
#3263 = CARTESIAN_POINT('',(-2.79508497187473,2.29621274840129E-15,18.75)) ;
#3264 = CARTESIAN_POINT('',(-2.79508497187473,-2.29621274840129E-15,-18.75)) ;
#3265 = CARTESIAN_POINT('Origin',(-2.79508497187473,0.,0.)) ;
#3266 = CARTESIAN_POINT('Origin',(0.,-2.60237444818813E-15,-21.25)) ;
#3267 = CARTESIAN_POINT('Origin',(-2.79508497187473,0.,0.)) ;
#3268 = CARTESIAN_POINT('Origin',(-5.5,0.,0.)) ;
#3269 = CARTESIAN_POINT('',(-6.5,-1.95943487863577E-15,16.)) ;
#3270 = CARTESIAN_POINT('Origin',(-6.5,0.,0.)) ;
#3271 = CARTESIAN_POINT('',(-5.5,-1.83697019872103E-15,15.)) ;
#3272 = CARTESIAN_POINT('Origin',(-5.5,-1.95943487863577E-15,16.)) ;
#3273 = CARTESIAN_POINT('Origin',(-5.5,0.,0.)) ;
#3274 = CARTESIAN_POINT('Origin',(-20.6375,0.,0.)) ;
#3275 = CARTESIAN_POINT('',(5.5,-1.83697019872103E-15,15.)) ;
#3276 = CARTESIAN_POINT('',(-20.6375,-1.83697019872103E-15,15.)) ;
#3277 = CARTESIAN_POINT('Origin',(5.5,0.,0.)) ;
#3278 = CARTESIAN_POINT('Origin',(5.5,0.,0.)) ;
#3279 = CARTESIAN_POINT('',(6.5,-1.95943487863577E-15,16.)) ;
#3280 = CARTESIAN_POINT('Origin',(5.5,-1.95943487863577E-15,16.)) ;
#3281 = CARTESIAN_POINT('Origin',(6.5,0.,0.)) ;
#3282 = CARTESIAN_POINT('Origin',(-20.6375,0.,0.)) ;
#3283 = CARTESIAN_POINT('',(-6.5,-2.29621274840129E-15,18.75)) ;
#3284 = CARTESIAN_POINT('',(-20.6375,-2.29621274840129E-15,18.75)) ;
#3285 = CARTESIAN_POINT('Origin',(-6.5,0.,0.)) ;
#3286 = CARTESIAN_POINT('Origin',(-20.6375,0.,0.)) ;
#3287 = CARTESIAN_POINT('',(6.5,-2.29621274840129E-15,18.75)) ;
#3288 = CARTESIAN_POINT('Origin',(6.5,0.,0.)) ;
#3289 = CARTESIAN_POINT('',(2.79508497187473,-2.29621274840129E-15,18.75)) ;
#3290 = CARTESIAN_POINT('',(-20.6375,-2.29621274840129E-15,18.75)) ;
#3291 = CARTESIAN_POINT('',(2.79508497187473,2.60237444818813E-15,-18.75)) ;
#3292 = CARTESIAN_POINT('Origin',(2.79508497187473,0.,0.)) ;
#3293 = CARTESIAN_POINT('Origin',(2.79508497187473,0.,0.)) ;
#3294 = CARTESIAN_POINT('Origin',(0.,0.,0.)) ;
#3295 = CARTESIAN_POINT('Origin',(0.,-2.60237444818813E-15,-21.25)) ;
#3296 = CARTESIAN_POINT('Origin',(6.5,16.,0.)) ;
#3297 = CARTESIAN_POINT('Origin',(-6.5,18.75,0.)) ;
#3298 = CARTESIAN_POINT('Origin',(6.5,26.5,0.)) ;
#3299 = CARTESIAN_POINT('Origin',(-6.5,23.75,0.)) ;
#3300 = CARTESIAN_POINT('',(0.,0.,0.)) ;
#3301 = CARTESIAN_POINT('Origin',(5.7,0.,0.)) ;
#3302 = CARTESIAN_POINT('',(5.7,4.89858719658941E-16,-4.)) ;
#3303 = CARTESIAN_POINT('',(5.7,-4.89858719658941E-16,4.)) ;
#3304 = CARTESIAN_POINT('Origin',(5.7,0.,0.)) ;
#3305 = CARTESIAN_POINT('Origin',(5.7,0.,0.)) ;
#3306 = CARTESIAN_POINT('',(5.3,-5.38844591624835E-16,4.4)) ;
#3307 = CARTESIAN_POINT('Origin',(5.7,-5.38844591624835E-16,4.4)) ;
#3308 = CARTESIAN_POINT('Origin',(5.3,0.,0.)) ;
#3309 = CARTESIAN_POINT('Origin',(0.,0.,0.)) ;
#3310 = CARTESIAN_POINT('',(4.7,5.62916512459884,-3.25000000000001)) ;
#3311 = CARTESIAN_POINT('',(4.7,1.50231459873716E-15,-6.5)) ;
#3312 = CARTESIAN_POINT('Origin',(4.7,0.,0.)) ;
#3313 = CARTESIAN_POINT('',(4.7,5.62916512459885,3.25)) ;
#3314 = CARTESIAN_POINT('Origin',(4.7,0.,0.)) ;
#3315 = CARTESIAN_POINT('',(4.7,0.,6.5)) ;
#3316 = CARTESIAN_POINT('Origin',(4.7,0.,0.)) ;
#3317 = CARTESIAN_POINT('',(4.7,-5.62916512459884,3.25000000000001)) ;
#3318 = CARTESIAN_POINT('Origin',(4.7,0.,0.)) ;
#3319 = CARTESIAN_POINT('',(4.7,-5.62916512459885,-3.25)) ;
#3320 = CARTESIAN_POINT('Origin',(4.7,0.,0.)) ;
#3321 = CARTESIAN_POINT('Origin',(4.7,0.,0.)) ;
#3322 = CARTESIAN_POINT('',(5.3,-7.96020419445779E-16,-6.5)) ;
#3323 = CARTESIAN_POINT('',(0.,-7.9602041944578E-16,-6.5)) ;
#3324 = CARTESIAN_POINT('Origin',(5.3,0.,0.)) ;
#3325 = CARTESIAN_POINT('Origin',(40.3,0.,0.)) ;
#3326 = CARTESIAN_POINT('',(39.6095,-4.89858719658941E-16,-4.)) ;
#3327 = CARTESIAN_POINT('Origin',(39.6095,0.,0.)) ;
#3328 = CARTESIAN_POINT('',(40.3,-4.05296858177817E-16,-3.3095)) ;
#3329 = CARTESIAN_POINT('',(40.3,-4.05296858177817E-16,-3.3095)) ;
#3330 = CARTESIAN_POINT('Origin',(40.3,0.,0.)) ;
#3331 = CARTESIAN_POINT('Origin',(0.,0.,0.)) ;
#3332 = CARTESIAN_POINT('',(0.,-4.89858719658941E-16,-4.)) ;
#3333 = CARTESIAN_POINT('Origin',(5.3,7.50555349946514,-6.50521303491302E-16)) ;
#3334 = CARTESIAN_POINT('Origin',(40.3,0.,0.)) ;
#3335 = CARTESIAN_POINT('Origin',(4.7,6.5,0.)) ;
#3336 = CARTESIAN_POINT('',(4.7,3.75277674973255,-6.5)) ;
#3337 = CARTESIAN_POINT('',(4.7,3.75277674973255,-6.5)) ;
#3338 = CARTESIAN_POINT('',(4.7,3.75277674973255,-6.5)) ;
#3339 = CARTESIAN_POINT('Origin',(4.7,6.5,0.)) ;
#3340 = CARTESIAN_POINT('',(4.7,7.50555349946514,0.)) ;
#3341 = CARTESIAN_POINT('',(4.7,3.75277674973255,-6.5)) ;
#3342 = CARTESIAN_POINT('',(4.7,7.50555349946514,0.)) ;
#3343 = CARTESIAN_POINT('Origin',(4.7,6.5,0.)) ;
#3344 = CARTESIAN_POINT('',(4.7,3.75277674973257,6.5)) ;
#3345 = CARTESIAN_POINT('',(4.7,7.50555349946514,0.)) ;
#3346 = CARTESIAN_POINT('',(4.7,3.75277674973257,6.5)) ;
#3347 = CARTESIAN_POINT('Origin',(4.7,6.5,0.)) ;
#3348 = CARTESIAN_POINT('',(4.7,-3.75277674973255,6.5)) ;
#3349 = CARTESIAN_POINT('',(4.7,3.75277674973257,6.5)) ;
#3350 = CARTESIAN_POINT('',(4.7,-7.50555349946514,3.54642105489778E-16)) ;
#3351 = CARTESIAN_POINT('Origin',(4.7,6.5,0.)) ;
#3352 = CARTESIAN_POINT('',(4.7,-7.50555349946514,0.)) ;
#3353 = CARTESIAN_POINT('',(4.7,-7.50555349946514,3.54642105489778E-16)) ;
#3354 = CARTESIAN_POINT('',(4.7,-3.75277674973258,-6.5)) ;
#3355 = CARTESIAN_POINT('Origin',(4.7,6.5,0.)) ;
#3356 = CARTESIAN_POINT('',(4.7,-3.75277674973258,-6.5)) ;
#3357 = CARTESIAN_POINT('',(4.7,-3.75277674973258,-6.5)) ;
#3358 = CARTESIAN_POINT('',(4.7,3.75277674973255,-6.5)) ;
#3359 = CARTESIAN_POINT('Origin',(0.,7.50555349946514,-6.50521303491302E-16)) ;
#3360 = CARTESIAN_POINT('',(0.,1.50231459873716E-15,-6.5)) ;
#3361 = CARTESIAN_POINT('',(0.,5.62916512459884,-3.25000000000001)) ;
#3362 = CARTESIAN_POINT('Origin',(0.,0.,0.)) ;
#3363 = CARTESIAN_POINT('',(0.,-5.62916512459885,-3.24999999999999)) ;
#3364 = CARTESIAN_POINT('Origin',(0.,0.,0.)) ;
#3365 = CARTESIAN_POINT('',(0.,-5.62916512459884,3.25000000000001)) ;
#3366 = CARTESIAN_POINT('Origin',(0.,0.,0.)) ;
#3367 = CARTESIAN_POINT('',(0.,1.50231459873716E-15,6.5)) ;
#3368 = CARTESIAN_POINT('Origin',(0.,0.,0.)) ;
#3369 = CARTESIAN_POINT('',(0.,5.62916512459885,3.25)) ;
#3370 = CARTESIAN_POINT('Origin',(0.,0.,0.)) ;
#3371 = CARTESIAN_POINT('Origin',(0.,0.,0.)) ;
#3372 = CARTESIAN_POINT('Origin',(0.,0.,0.)) ;
#3373 = CARTESIAN_POINT('',(0.580556583600765,7.50555349946514,1.86597838430726E-16)) ;
#3374 = CARTESIAN_POINT('Ctrl Pts',(2.52404060397759E-15,5.62916512459885,
3.25000000000001)) ;
#3375 = CARTESIAN_POINT('Ctrl Pts',(1.94289029309402E-15,6.50000000000069,
1.7416697508011)) ;
#3376 = CARTESIAN_POINT('Ctrl Pts',(0.58055658360176,7.50555349946686,-2.98168594117076E-12)) ;
#3377 = CARTESIAN_POINT('Ctrl Pts',(0.58055658360176,7.50555349946686,2.98331750666524E-12)) ;
#3378 = CARTESIAN_POINT('Ctrl Pts',(-1.12537942179479E-15,6.50000000000069,
-1.7416697508011)) ;
#3379 = CARTESIAN_POINT('Ctrl Pts',(-1.13581827178992E-15,5.62916512459884,
-3.25000000000001)) ;
#3380 = CARTESIAN_POINT('Origin',(0.,0.,0.)) ;
#3381 = CARTESIAN_POINT('',(0.580556583600762,3.75277674973257,6.5)) ;
#3382 = CARTESIAN_POINT('Ctrl Pts',(1.13581827178992E-15,2.52404060397759E-15,
6.5)) ;
#3383 = CARTESIAN_POINT('Ctrl Pts',(1.2490009027033E-15,1.74166975080368,
6.5)) ;
#3384 = CARTESIAN_POINT('Ctrl Pts',(0.580556583601757,3.75277674973601,6.5)) ;
#3385 = CARTESIAN_POINT('Ctrl Pts',(0.580556583601759,3.75277674973085,6.50000000000299)) ;
#3386 = CARTESIAN_POINT('Ctrl Pts',(3.30581563765696E-15,4.75833024919701,
4.75833024919891)) ;
#3387 = CARTESIAN_POINT('Ctrl Pts',(2.52404060397759E-15,5.62916512459885,
3.25000000000001)) ;
#3388 = CARTESIAN_POINT('Origin',(0.,0.,0.)) ;
#3389 = CARTESIAN_POINT('',(0.580556583600758,-3.75277674973255,6.5)) ;
#3390 = CARTESIAN_POINT('Ctrl Pts',(0.580556583601755,-3.752776749736,6.5)) ;
#3391 = CARTESIAN_POINT('Ctrl Pts',(1.12537942179479E-15,-1.74166975080368,
6.5)) ;
#3392 = CARTESIAN_POINT('Ctrl Pts',(1.13581827178992E-15,2.52404060397759E-15,
6.5)) ;
#3393 = CARTESIAN_POINT('Ctrl Pts',(0.,-5.62916512459884,3.25000000000001)) ;
#3394 = CARTESIAN_POINT('Ctrl Pts',(2.77555756156289E-16,-4.758330249197,
4.75833024919891)) ;
#3395 = CARTESIAN_POINT('Ctrl Pts',(0.580556583601755,-3.75277674973083,6.50000000000299)) ;
#3396 = CARTESIAN_POINT('Origin',(0.,0.,0.)) ;
#3397 = CARTESIAN_POINT('',(0.580556583600765,-7.50555349946514,-1.19038851851474E-16)) ;
#3398 = CARTESIAN_POINT('Ctrl Pts',(0.580556583601757,-7.50555349946686,-2.97026498270936E-12)) ;
#3399 = CARTESIAN_POINT('Ctrl Pts',(0.,-6.50000000000069,1.74166975080111)) ;
#3400 = CARTESIAN_POINT('Ctrl Pts',(0.,-5.62916512459884,3.25000000000001)) ;
#3401 = CARTESIAN_POINT('Ctrl Pts',(5.42668729855182E-15,-5.62916512459886,
-3.25)) ;
#3402 = CARTESIAN_POINT('Ctrl Pts',(4.92661467177413E-15,-6.5000000000007,
-1.7416697508011)) ;
#3403 = CARTESIAN_POINT('Ctrl Pts',(0.58055658360176,-7.50555349946686,2.97923859292903E-12)) ;
#3404 = CARTESIAN_POINT('Origin',(0.,0.,0.)) ;
#3405 = CARTESIAN_POINT('',(0.580556583600758,3.75277674973255,-6.5)) ;
#3406 = CARTESIAN_POINT('Ctrl Pts',(-1.13581827178992E-15,5.62916512459884,
-3.25000000000001)) ;
#3407 = CARTESIAN_POINT('Ctrl Pts',(-1.04083408558608E-15,4.758330249197,
-4.75833024919891)) ;
#3408 = CARTESIAN_POINT('Ctrl Pts',(0.580556583601754,3.75277674973083,-6.50000000000299)) ;
#3409 = CARTESIAN_POINT('Ctrl Pts',(0.58055658360175,3.75277674973599,-6.5)) ;
#3410 = CARTESIAN_POINT('Ctrl Pts',(3.103447877054E-16,1.74166975080367,-6.5)) ;
#3411 = CARTESIAN_POINT('Ctrl Pts',(1.13581827178992E-15,-2.01923248318207E-15,
-6.5)) ;
#3412 = CARTESIAN_POINT('Origin',(0.,0.,0.)) ;
#3413 = CARTESIAN_POINT('',(0.580556583600767,-3.75277674973258,-6.5)) ;
#3414 = CARTESIAN_POINT('Ctrl Pts',(0.580556583601764,-3.75277674973085,-6.50000000000299)) ;
#3415 = CARTESIAN_POINT('Ctrl Pts',(6.02079077550993E-15,-4.75833024919702,
-4.75833024919891)) ;
#3416 = CARTESIAN_POINT('Ctrl Pts',(5.42668729855182E-15,-5.62916512459886,
-3.25)) ;
#3417 = CARTESIAN_POINT('Ctrl Pts',(1.13581827178992E-15,-2.01923248318207E-15,
-6.5)) ;
#3418 = CARTESIAN_POINT('Ctrl Pts',(2.15105711021124E-15,-1.74166975080369,
-6.5)) ;
#3419 = CARTESIAN_POINT('Ctrl Pts',(0.580556583601762,-3.75277674973603,-6.5)) ;
#3420 = CARTESIAN_POINT('Origin',(5.3,3.75277674973255,-6.5)) ;
#3421 = CARTESIAN_POINT('',(5.3,-3.75277674973258,-6.5)) ;
#3422 = CARTESIAN_POINT('',(5.3,3.75277674973255,-6.5)) ;
#3423 = CARTESIAN_POINT('Origin',(5.3,-3.75277674973258,-6.5)) ;
#3424 = CARTESIAN_POINT('',(5.3,-7.50555349946514,3.54642105489778E-16)) ;
#3425 = CARTESIAN_POINT('Origin',(5.3,-7.50555349946514,3.54642105489778E-16)) ;
#3426 = CARTESIAN_POINT('',(5.3,-3.75277674973255,6.5)) ;
#3427 = CARTESIAN_POINT('Origin',(5.3,3.75277674973257,6.5)) ;
#3428 = CARTESIAN_POINT('',(5.3,3.75277674973257,6.5)) ;
#3429 = CARTESIAN_POINT('Origin',(5.3,7.50555349946514,0.)) ;
#3430 = CARTESIAN_POINT('',(5.3,7.50555349946514,0.)) ;
#3431 = CARTESIAN_POINT('Origin',(5.3,3.75277674973255,-6.5)) ;
#3432 = CARTESIAN_POINT('',(-200.,251.533301909419,-44.9999999999981)) ;
#3433 = CARTESIAN_POINT('',(-300.,79.9999999999993,72.0000000000023)) ;
#3434 = CARTESIAN_POINT('',(-100.,79.9999999999999,71.9999999999987)) ;
#3435 = CARTESIAN_POINT('',(-200.,233.691743315451,71.9999999999999)) ;
#3436 = CARTESIAN_POINT('',(0.,0.,0.)) ;
#3437 = CARTESIAN_POINT('',(0.,0.,0.)) ;
#3438 = CARTESIAN_POINT('',(0.,0.,0.)) ;
#3439 = CARTESIAN_POINT('',(0.,0.,0.)) ;
#3440 = UNCERTAINTY_MEASURE_WITH_UNIT(LENGTH_MEASURE(0.01),#3476,
'DISTANCE_ACCURACY_VALUE',
'Maximum model space distance between geometric entities at asserted c
onnectivities') ;
#3441 = UNCERTAINTY_MEASURE_WITH_UNIT(LENGTH_MEASURE(0.01),#3476,
'DISTANCE_ACCURACY_VALUE',
'Maximum model space distance between geometric entities at asserted c
onnectivities') ;
#3442 = UNCERTAINTY_MEASURE_WITH_UNIT(LENGTH_MEASURE(0.01),#3476,
'DISTANCE_ACCURACY_VALUE',
'Maximum model space distance between geometric entities at asserted c
onnectivities') ;
#3443 = UNCERTAINTY_MEASURE_WITH_UNIT(LENGTH_MEASURE(0.01),#3476,
'DISTANCE_ACCURACY_VALUE',
'Maximum model space distance between geometric entities at asserted c
onnectivities') ;
#3444 = UNCERTAINTY_MEASURE_WITH_UNIT(LENGTH_MEASURE(0.01),#3476,
'DISTANCE_ACCURACY_VALUE',
'Maximum model space distance between geometric entities at asserted c
onnectivities') ;
#3445 = UNCERTAINTY_MEASURE_WITH_UNIT(LENGTH_MEASURE(0.01),#3476,
'DISTANCE_ACCURACY_VALUE',
'Maximum model space distance between geometric entities at asserted c
onnectivities') ;
#3446 = UNCERTAINTY_MEASURE_WITH_UNIT(LENGTH_MEASURE(0.01),#3476,
'DISTANCE_ACCURACY_VALUE',
'Maximum model space distance between geometric entities at asserted c
onnectivities') ;
#3447 = UNCERTAINTY_MEASURE_WITH_UNIT(LENGTH_MEASURE(0.01),#3476,
'DISTANCE_ACCURACY_VALUE',
'Maximum model space distance between geometric entities at asserted c
onnectivities') ;
#3448 = UNCERTAINTY_MEASURE_WITH_UNIT(LENGTH_MEASURE(0.01),#3476,
'DISTANCE_ACCURACY_VALUE',
'Maximum model space distance between geometric entities at asserted c
onnectivities') ;
#3449 = UNCERTAINTY_MEASURE_WITH_UNIT(LENGTH_MEASURE(0.01),#3476,
'DISTANCE_ACCURACY_VALUE',
'Maximum model space distance between geometric entities at asserted c
onnectivities') ;
#3450 = UNCERTAINTY_MEASURE_WITH_UNIT(LENGTH_MEASURE(0.01),#3476,
'DISTANCE_ACCURACY_VALUE',
'Maximum model space distance between geometric entities at asserted c
onnectivities') ;
#3451 = UNCERTAINTY_MEASURE_WITH_UNIT(LENGTH_MEASURE(0.01),#3476,
'DISTANCE_ACCURACY_VALUE',
'Maximum model space distance between geometric entities at asserted c
onnectivities') ;
#3452 = UNCERTAINTY_MEASURE_WITH_UNIT(LENGTH_MEASURE(0.01),#3476,
'DISTANCE_ACCURACY_VALUE',
'Maximum model space distance between geometric entities at asserted c
onnectivities') ;
#3453 = UNCERTAINTY_MEASURE_WITH_UNIT(LENGTH_MEASURE(0.01),#3476,
'DISTANCE_ACCURACY_VALUE',
'Maximum model space distance between geometric entities at asserted c
onnectivities') ;
#3454 = UNCERTAINTY_MEASURE_WITH_UNIT(LENGTH_MEASURE(0.01),#3476,
'DISTANCE_ACCURACY_VALUE',
'Maximum model space distance between geometric entities at asserted c
onnectivities') ;
#3455 = UNCERTAINTY_MEASURE_WITH_UNIT(LENGTH_MEASURE(0.01),#3476,
'DISTANCE_ACCURACY_VALUE',
'Maximum model space distance between geometric entities at asserted c
onnectivities') ;
#3456 = UNCERTAINTY_MEASURE_WITH_UNIT(LENGTH_MEASURE(0.01),#3476,
'DISTANCE_ACCURACY_VALUE',
'Maximum model space distance between geometric entities at asserted c
onnectivities') ;
#3457 = UNCERTAINTY_MEASURE_WITH_UNIT(LENGTH_MEASURE(0.01),#3476,
'DISTANCE_ACCURACY_VALUE',
'Maximum model space distance between geometric entities at asserted c
onnectivities') ;
#3458 = (
GEOMETRIC_REPRESENTATION_CONTEXT(3)
GLOBAL_UNCERTAINTY_ASSIGNED_CONTEXT((#3440))
GLOBAL_UNIT_ASSIGNED_CONTEXT((#3476,#3478,#3479))
REPRESENTATION_CONTEXT('','3D')
) ;
#3459 = (
GEOMETRIC_REPRESENTATION_CONTEXT(3)
GLOBAL_UNCERTAINTY_ASSIGNED_CONTEXT((#3441))
GLOBAL_UNIT_ASSIGNED_CONTEXT((#3476,#3478,#3479))
REPRESENTATION_CONTEXT('','3D')
) ;
#3460 = (
GEOMETRIC_REPRESENTATION_CONTEXT(3)
GLOBAL_UNCERTAINTY_ASSIGNED_CONTEXT((#3442))
GLOBAL_UNIT_ASSIGNED_CONTEXT((#3476,#3478,#3479))
REPRESENTATION_CONTEXT('','3D')
) ;
#3461 = (
GEOMETRIC_REPRESENTATION_CONTEXT(3)
GLOBAL_UNCERTAINTY_ASSIGNED_CONTEXT((#3443))
GLOBAL_UNIT_ASSIGNED_CONTEXT((#3476,#3478,#3479))
REPRESENTATION_CONTEXT('','3D')
) ;
#3462 = (
GEOMETRIC_REPRESENTATION_CONTEXT(3)
GLOBAL_UNCERTAINTY_ASSIGNED_CONTEXT((#3444))
GLOBAL_UNIT_ASSIGNED_CONTEXT((#3476,#3478,#3479))
REPRESENTATION_CONTEXT('','3D')
) ;
#3463 = (
GEOMETRIC_REPRESENTATION_CONTEXT(3)
GLOBAL_UNCERTAINTY_ASSIGNED_CONTEXT((#3445))
GLOBAL_UNIT_ASSIGNED_CONTEXT((#3476,#3478,#3479))
REPRESENTATION_CONTEXT('','3D')
) ;
#3464 = (
GEOMETRIC_REPRESENTATION_CONTEXT(3)
GLOBAL_UNCERTAINTY_ASSIGNED_CONTEXT((#3446))
GLOBAL_UNIT_ASSIGNED_CONTEXT((#3476,#3478,#3479))
REPRESENTATION_CONTEXT('','3D')
) ;
#3465 = (
GEOMETRIC_REPRESENTATION_CONTEXT(3)
GLOBAL_UNCERTAINTY_ASSIGNED_CONTEXT((#3447))
GLOBAL_UNIT_ASSIGNED_CONTEXT((#3476,#3478,#3479))
REPRESENTATION_CONTEXT('','3D')
) ;
#3466 = (
GEOMETRIC_REPRESENTATION_CONTEXT(3)
GLOBAL_UNCERTAINTY_ASSIGNED_CONTEXT((#3448))
GLOBAL_UNIT_ASSIGNED_CONTEXT((#3476,#3478,#3479))
REPRESENTATION_CONTEXT('','3D')
) ;
#3467 = (
GEOMETRIC_REPRESENTATION_CONTEXT(3)
GLOBAL_UNCERTAINTY_ASSIGNED_CONTEXT((#3449))
GLOBAL_UNIT_ASSIGNED_CONTEXT((#3476,#3478,#3479))
REPRESENTATION_CONTEXT('','3D')
) ;
#3468 = (
GEOMETRIC_REPRESENTATION_CONTEXT(3)
GLOBAL_UNCERTAINTY_ASSIGNED_CONTEXT((#3450))
GLOBAL_UNIT_ASSIGNED_CONTEXT((#3476,#3478,#3479))
REPRESENTATION_CONTEXT('','3D')
) ;
#3469 = (
GEOMETRIC_REPRESENTATION_CONTEXT(3)
GLOBAL_UNCERTAINTY_ASSIGNED_CONTEXT((#3451))
GLOBAL_UNIT_ASSIGNED_CONTEXT((#3476,#3478,#3479))
REPRESENTATION_CONTEXT('','3D')
) ;
#3470 = (
GEOMETRIC_REPRESENTATION_CONTEXT(3)
GLOBAL_UNCERTAINTY_ASSIGNED_CONTEXT((#3452))
GLOBAL_UNIT_ASSIGNED_CONTEXT((#3476,#3478,#3479))
REPRESENTATION_CONTEXT('','3D')
) ;
#3471 = (
GEOMETRIC_REPRESENTATION_CONTEXT(3)
GLOBAL_UNCERTAINTY_ASSIGNED_CONTEXT((#3453))
GLOBAL_UNIT_ASSIGNED_CONTEXT((#3476,#3478,#3479))
REPRESENTATION_CONTEXT('','3D')
) ;
#3472 = (
GEOMETRIC_REPRESENTATION_CONTEXT(3)
GLOBAL_UNCERTAINTY_ASSIGNED_CONTEXT((#3454))
GLOBAL_UNIT_ASSIGNED_CONTEXT((#3476,#3478,#3479))
REPRESENTATION_CONTEXT('','3D')
) ;
#3473 = (
GEOMETRIC_REPRESENTATION_CONTEXT(3)
GLOBAL_UNCERTAINTY_ASSIGNED_CONTEXT((#3455))
GLOBAL_UNIT_ASSIGNED_CONTEXT((#3476,#3478,#3479))
REPRESENTATION_CONTEXT('','3D')
) ;
#3474 = (
GEOMETRIC_REPRESENTATION_CONTEXT(3)
GLOBAL_UNCERTAINTY_ASSIGNED_CONTEXT((#3456))
GLOBAL_UNIT_ASSIGNED_CONTEXT((#3476,#3478,#3479))
REPRESENTATION_CONTEXT('','3D')
) ;
#3475 = (
GEOMETRIC_REPRESENTATION_CONTEXT(3)
GLOBAL_UNCERTAINTY_ASSIGNED_CONTEXT((#3457))
GLOBAL_UNIT_ASSIGNED_CONTEXT((#3476,#3478,#3479))
REPRESENTATION_CONTEXT('','3D')
) ;
#3476 = (
LENGTH_UNIT()
NAMED_UNIT(*)
SI_UNIT(.MILLI.,.METRE.)
) ;
#3477 = (
LENGTH_UNIT()
NAMED_UNIT(*)
SI_UNIT($,.METRE.)
) ;
#3478 = (
NAMED_UNIT(*)
PLANE_ANGLE_UNIT()
SI_UNIT($,.RADIAN.)
) ;
#3479 = (
NAMED_UNIT(*)
SI_UNIT($,.STERADIAN.)
SOLID_ANGLE_UNIT()
) ;
#3480 = SHAPE_DEFINITION_REPRESENTATION(#3497,#3538) ;
#3481 = SHAPE_DEFINITION_REPRESENTATION(#3498,#3539) ;
#3482 = SHAPE_DEFINITION_REPRESENTATION(#3499,#3540) ;
#3483 = SHAPE_DEFINITION_REPRESENTATION(#3500,#3541) ;
#3484 = SHAPE_DEFINITION_REPRESENTATION(#3501,#3542) ;
#3485 = SHAPE_DEFINITION_REPRESENTATION(#3506,#3543) ;
#3486 = SHAPE_DEFINITION_REPRESENTATION(#3507,#3544) ;
#3487 = SHAPE_DEFINITION_REPRESENTATION(#3508,#3545) ;
#3488 = SHAPE_DEFINITION_REPRESENTATION(#3509,#3546) ;
#3489 = SHAPE_DEFINITION_REPRESENTATION(#3510,#3547) ;
#3490 = SHAPE_DEFINITION_REPRESENTATION(#3511,#3548) ;
#3491 = SHAPE_DEFINITION_REPRESENTATION(#3518,#3549) ;
#3492 = SHAPE_DEFINITION_REPRESENTATION(#3519,#3550) ;
#3493 = SHAPE_DEFINITION_REPRESENTATION(#3520,#3551) ;
#3494 = SHAPE_DEFINITION_REPRESENTATION(#3527,#3552) ;
#3495 = SHAPE_DEFINITION_REPRESENTATION(#3528,#3553) ;
#3496 = SHAPE_DEFINITION_REPRESENTATION(#3529,#3554) ;
#3497 = PRODUCT_DEFINITION_SHAPE('',$,#3556) ;
#3498 = PRODUCT_DEFINITION_SHAPE('',$,#3557) ;
#3499 = PRODUCT_DEFINITION_SHAPE('',$,#3558) ;
#3500 = PRODUCT_DEFINITION_SHAPE('',$,#3559) ;
#3501 = PRODUCT_DEFINITION_SHAPE('',$,#3560) ;
#3502 = PRODUCT_DEFINITION_SHAPE($,$,#117) ;
#3503 = PRODUCT_DEFINITION_SHAPE($,$,#118) ;
#3504 = PRODUCT_DEFINITION_SHAPE($,$,#119) ;
#3505 = PRODUCT_DEFINITION_SHAPE($,$,#120) ;
#3506 = PRODUCT_DEFINITION_SHAPE('',$,#3561) ;
#3507 = PRODUCT_DEFINITION_SHAPE('',$,#3562) ;
#3508 = PRODUCT_DEFINITION_SHAPE('',$,#3563) ;
#3509 = PRODUCT_DEFINITION_SHAPE('',$,#3564) ;
#3510 = PRODUCT_DEFINITION_SHAPE('',$,#3565) ;
#3511 = PRODUCT_DEFINITION_SHAPE('',$,#3566) ;
#3512 = PRODUCT_DEFINITION_SHAPE($,$,#121) ;
#3513 = PRODUCT_DEFINITION_SHAPE($,$,#122) ;
#3514 = PRODUCT_DEFINITION_SHAPE($,$,#123) ;
#3515 = PRODUCT_DEFINITION_SHAPE($,$,#124) ;
#3516 = PRODUCT_DEFINITION_SHAPE($,$,#125) ;
#3517 = PRODUCT_DEFINITION_SHAPE($,$,#126) ;
#3518 = PRODUCT_DEFINITION_SHAPE('',$,#3567) ;
#3519 = PRODUCT_DEFINITION_SHAPE('',$,#3568) ;
#3520 = PRODUCT_DEFINITION_SHAPE('',$,#3569) ;
#3521 = PRODUCT_DEFINITION_SHAPE($,$,#127) ;
#3522 = PRODUCT_DEFINITION_SHAPE($,$,#128) ;
#3523 = PRODUCT_DEFINITION_SHAPE($,$,#129) ;
#3524 = PRODUCT_DEFINITION_SHAPE($,$,#130) ;
#3525 = PRODUCT_DEFINITION_SHAPE($,$,#131) ;
#3526 = PRODUCT_DEFINITION_SHAPE($,$,#132) ;
#3527 = PRODUCT_DEFINITION_SHAPE('',$,#3570) ;
#3528 = PRODUCT_DEFINITION_SHAPE('',$,#3571) ;
#3529 = PRODUCT_DEFINITION_SHAPE('',$,#3572) ;
#3530 = PRODUCT_DEFINITION_SHAPE($,$,#133) ;
#3531 = PRODUCT_DEFINITION_SHAPE($,$,#134) ;
#3532 = PRODUCT_DEFINITION_SHAPE($,$,#135) ;
#3533 = PRODUCT_DEFINITION_SHAPE($,$,#136) ;
#3534 = PRODUCT_DEFINITION_SHAPE($,$,#137) ;
#3535 = PRODUCT_DEFINITION_SHAPE($,$,#138) ;
#3536 = PRODUCT_DEFINITION_SHAPE($,$,#139) ;
#3537 = PRODUCT_DEFINITION_SHAPE($,$,#140) ;
#3538 = SHAPE_REPRESENTATION('',(#1969,#2210,#2211,#2212,#2213),#3458) ;
#3539 = SHAPE_REPRESENTATION('',(#1970,#2007,#2008,#2009,#2010),#3459) ;
#3540 = SHAPE_REPRESENTATION('',(#1971),#3460) ;
#3541 = SHAPE_REPRESENTATION('',(#1978),#3461) ;
#3542 = SHAPE_REPRESENTATION('',(#1988),#3462) ;
#3543 = SHAPE_REPRESENTATION('',(#2011,#2079,#2080,#2081,#2082,#2083,#2084),
#3463) ;
#3544 = SHAPE_REPRESENTATION('',(#2012),#3464) ;
#3545 = SHAPE_REPRESENTATION('',(#2023),#3465) ;
#3546 = SHAPE_REPRESENTATION('',(#2029),#3466) ;
#3547 = SHAPE_REPRESENTATION('',(#2043),#3467) ;
#3548 = SHAPE_REPRESENTATION('',(#2061),#3468) ;
#3549 = SHAPE_REPRESENTATION('',(#2085,#2111,#2112,#2113,#2114,#2115,#2116),
#3469) ;
#3550 = SHAPE_REPRESENTATION('',(#2086),#3470) ;
#3551 = SHAPE_REPRESENTATION('',(#2102),#3471) ;
#3552 = SHAPE_REPRESENTATION('',(#2117,#2206,#2207,#2208,#2209),#3472) ;
#3553 = SHAPE_REPRESENTATION('',(#2118),#3473) ;
#3554 = SHAPE_REPRESENTATION('',(#2161),#3474) ;
#3555 = PRODUCT_DEFINITION_CONTEXT('part definition',#3608,'design') ;
#3556 = PRODUCT_DEFINITION('MAS-648',
'MAS-648',#3573,#3555) ;
#3557 = PRODUCT_DEFINITION('Plates','Plates',#3574,#3555) ;
#3558 = PRODUCT_DEFINITION('Lower_Feed_Plate','Lower_Feed_Plate',#3575,#3555) ;
#3559 = PRODUCT_DEFINITION('Middle_Plate',
'Middle_Plate',#3576,#3555) ;
#3560 = PRODUCT_DEFINITION('Main_Plate',
'Main_Plate',#3577,#3555) ;
#3561 = PRODUCT_DEFINITION('Bending_Mechanism','Bending_Mechanism',
#3578,#3555) ;
#3562 = PRODUCT_DEFINITION('Threaded_Drive_Shaft','Threaded_Drive_Shaft',#3579,#3555) ;
#3563 = PRODUCT_DEFINITION('Shaft','Shaft',#3580,#3555) ;
#3564 = PRODUCT_DEFINITION('Pivot_Mechanism','Pivot_Mechanism',#3581,#3555) ;
#3565 = PRODUCT_DEFINITION('Fixed_Fixture','Fixed_Fixture',#3582,#3555) ;
#3566 = PRODUCT_DEFINITION(
'Fixed_Fixture_Lower',
'Fixed_Fixture_Lower',#3583,#3555) ;
#3567 = PRODUCT_DEFINITION('Bending_Parts','Bending_Parts',#3584,
#3555) ;
#3568 = PRODUCT_DEFINITION('Bending_Part',
'Bending_Part',#3585,#3555) ;
#3569 = PRODUCT_DEFINITION('Washer',
'Washer',#3586,#3555) ;
#3570 = PRODUCT_DEFINITION('Hardware','Hardware',#3587,#3555) ;
#3571 = PRODUCT_DEFINITION('Ball_Bearing',
'Ball_Bearing',#3588,#3555) ;
#3572 = PRODUCT_DEFINITION('Hex_Screw_M8x35',
'Hex_Screw_M8x35',#3589,#3555) ;
#3573 = PRODUCT_DEFINITION_FORMATION('',$,#3610) ;
#3574 = PRODUCT_DEFINITION_FORMATION('',$,#3611) ;
#3575 = PRODUCT_DEFINITION_FORMATION('',$,#3612) ;
#3576 = PRODUCT_DEFINITION_FORMATION('',$,#3613) ;
#3577 = PRODUCT_DEFINITION_FORMATION('',$,#3614) ;
#3578 = PRODUCT_DEFINITION_FORMATION('',$,#3615) ;
#3579 = PRODUCT_DEFINITION_FORMATION('',$,#3616) ;
#3580 = PRODUCT_DEFINITION_FORMATION('',$,#3617) ;
#3581 = PRODUCT_DEFINITION_FORMATION('',$,#3618) ;
#3582 = PRODUCT_DEFINITION_FORMATION('',$,#3619) ;
#3583 = PRODUCT_DEFINITION_FORMATION('',$,#3620) ;
#3584 = PRODUCT_DEFINITION_FORMATION('',$,#3621) ;
#3585 = PRODUCT_DEFINITION_FORMATION('',$,#3622) ;
#3586 = PRODUCT_DEFINITION_FORMATION('',$,#3623) ;
#3587 = PRODUCT_DEFINITION_FORMATION('',$,#3624) ;
#3588 = PRODUCT_DEFINITION_FORMATION('',$,#3625) ;
#3589 = PRODUCT_DEFINITION_FORMATION('',$,#3626) ;
#3590 = PRODUCT_RELATED_PRODUCT_CATEGORY('MAS-648','MAS-648',(#3610)) ;
#3591 = PRODUCT_RELATED_PRODUCT_CATEGORY('Plates','Plates',(#3611)) ;
#3592 = PRODUCT_RELATED_PRODUCT_CATEGORY('Lower_Feed_Plate',
'Lower_Feed_Plate',(#3612)) ;
#3593 = PRODUCT_RELATED_PRODUCT_CATEGORY('Middle_Plate','Middle_Plate',(#3613)) ;
#3594 = PRODUCT_RELATED_PRODUCT_CATEGORY('Main_Plate','Main_Plate',(#3614)) ;
#3595 = PRODUCT_RELATED_PRODUCT_CATEGORY('Bending_Mechanism',
'Bending_Mechanism',(#3615)) ;
#3596 = PRODUCT_RELATED_PRODUCT_CATEGORY('Threaded_Drive_Shaft',
'Threaded_Drive_Shaft',(#3616)) ;
#3597 = PRODUCT_RELATED_PRODUCT_CATEGORY('Shaft','Shaft',(#3617)) ;
#3598 = PRODUCT_RELATED_PRODUCT_CATEGORY('Pivot_Mechanism',
'Pivot_Mechanism',(#3618)) ;
#3599 = PRODUCT_RELATED_PRODUCT_CATEGORY('Fixed_Fixture','Fixed_Fixture',
(#3619)) ;
#3600 = PRODUCT_RELATED_PRODUCT_CATEGORY('Fixed_Fixture_Lower',
'Fixed_Fixture_Lower',(#3620)) ;
#3601 = PRODUCT_RELATED_PRODUCT_CATEGORY('Bending_Parts','Bending_Parts',
(#3621)) ;
#3602 = PRODUCT_RELATED_PRODUCT_CATEGORY('Bending_Part','Bending_Part',(#3622)) ;
#3603 = PRODUCT_RELATED_PRODUCT_CATEGORY('Washer','Washer',(#3623)) ;
#3604 = PRODUCT_RELATED_PRODUCT_CATEGORY('Hardware','Hardware',(#3624)) ;
#3605 = PRODUCT_RELATED_PRODUCT_CATEGORY('Ball_Bearing','Ball_Bearing',(#3625)) ;
#3606 = PRODUCT_RELATED_PRODUCT_CATEGORY('Hex_Screw_M8x35',
'Hex_Screw_M8x35',(#3626)) ;
#3607 = APPLICATION_PROTOCOL_DEFINITION('international standard',
'automotive_design',2009,#3608) ;
#3608 = APPLICATION_CONTEXT(
'Core Data for Automotive Mechanical Design Process') ;
#3609 = PRODUCT_CONTEXT('part definition',#3608,'mechanical') ;
#3610 = PRODUCT('MAS-648','MAS-648',
'',(#3609)) ;
#3611 = PRODUCT('Plates','Plates',$,(#3609)) ;
#3612 = PRODUCT('Lower_Feed_Plate',
'Lower_Feed_Plate',$,(#3609)) ;
#3613 = PRODUCT('Middle_Plate',
'Middle_Plate',$,(#3609)) ;
#3614 = PRODUCT('Main_Plate','Main_Plate',
$,(#3609)) ;
#3615 = PRODUCT('Bending_Mechanism','Bending_Mechanism',$,(#3609)) ;
#3616 = PRODUCT('Threaded_Drive_Shaft','Threaded_Drive_Shaft',$,(#3609)) ;
#3617 = PRODUCT('Shaft',
'Shaft',$,(#3609)) ;
#3618 = PRODUCT('Pivot_Mechanism',
'Pivot_Mechanism',$,(#3609)) ;
#3619 = PRODUCT('Fixed_Fixture',
'Fixed_Fixture',$,(#3609)) ;
#3620 = PRODUCT('Fixed_Fixture_Lower',
'Fixed_Fixture_Lower',$,(#3609)) ;
#3621 = PRODUCT('Bending_Parts','Bending_Parts',$,(#3609)) ;
#3622 = PRODUCT('Bending_Part','Bending_Part',$,
(#3609)) ;
#3623 = PRODUCT('Washer','Washer',$,(#3609)) ;
#3624 = PRODUCT('Hardware','Hardware',$,(#3609)) ;
#3625 = PRODUCT('Ball_Bearing','Ball_Bearing',
$,(#3609)) ;
#3626 = PRODUCT('Hex_Screw_M8x35',
'Hex_Screw_M8x35',$,(#3609)) ;
#3627 = PRESENTATION_STYLE_ASSIGNMENT((#3629)) ;
#3628 = PRESENTATION_STYLE_ASSIGNMENT((#3630)) ;
#3629 = SURFACE_STYLE_USAGE(.BOTH.,#3631) ;
#3630 = SURFACE_STYLE_USAGE(.BOTH.,#3632) ;
#3631 = SURFACE_SIDE_STYLE('',(#3633)) ;
#3632 = SURFACE_SIDE_STYLE('',(#3634)) ;
#3633 = SURFACE_STYLE_FILL_AREA(#3635) ;
#3634 = SURFACE_STYLE_FILL_AREA(#3636) ;
#3635 = FILL_AREA_STYLE('Steel - Satin',(#3637)) ;
#3636 = FILL_AREA_STYLE('Opaque(202,209,238)',(#3638)) ;
#3637 = FILL_AREA_STYLE_COLOUR('Steel - Satin',#3639) ;
#3638 = FILL_AREA_STYLE_COLOUR('Opaque(202,209,238)',#3640) ;
#3639 = COLOUR_RGB('Steel - Satin', 0.09019608, 0.27058824, 0.51372549) ;
#3640 = COLOUR_RGB('Opaque(202,209,238)', 0.09019608, 0.27058824, 0.51372549) ;
ENDSEC;
END-ISO-10303-21;
